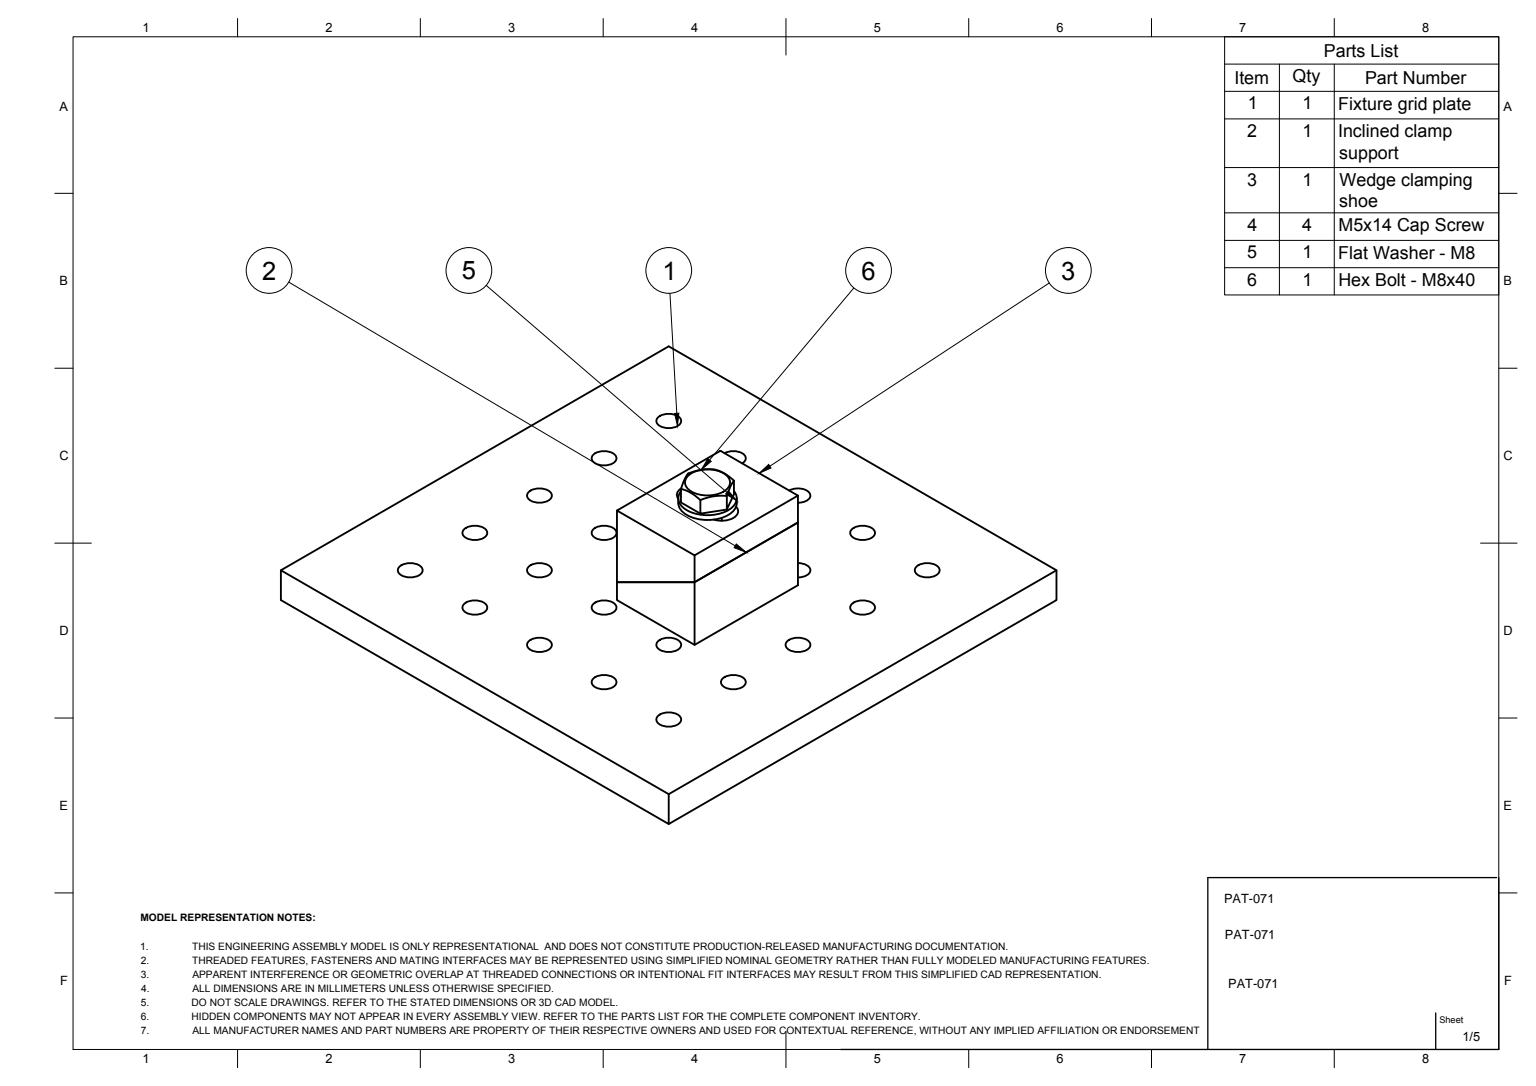
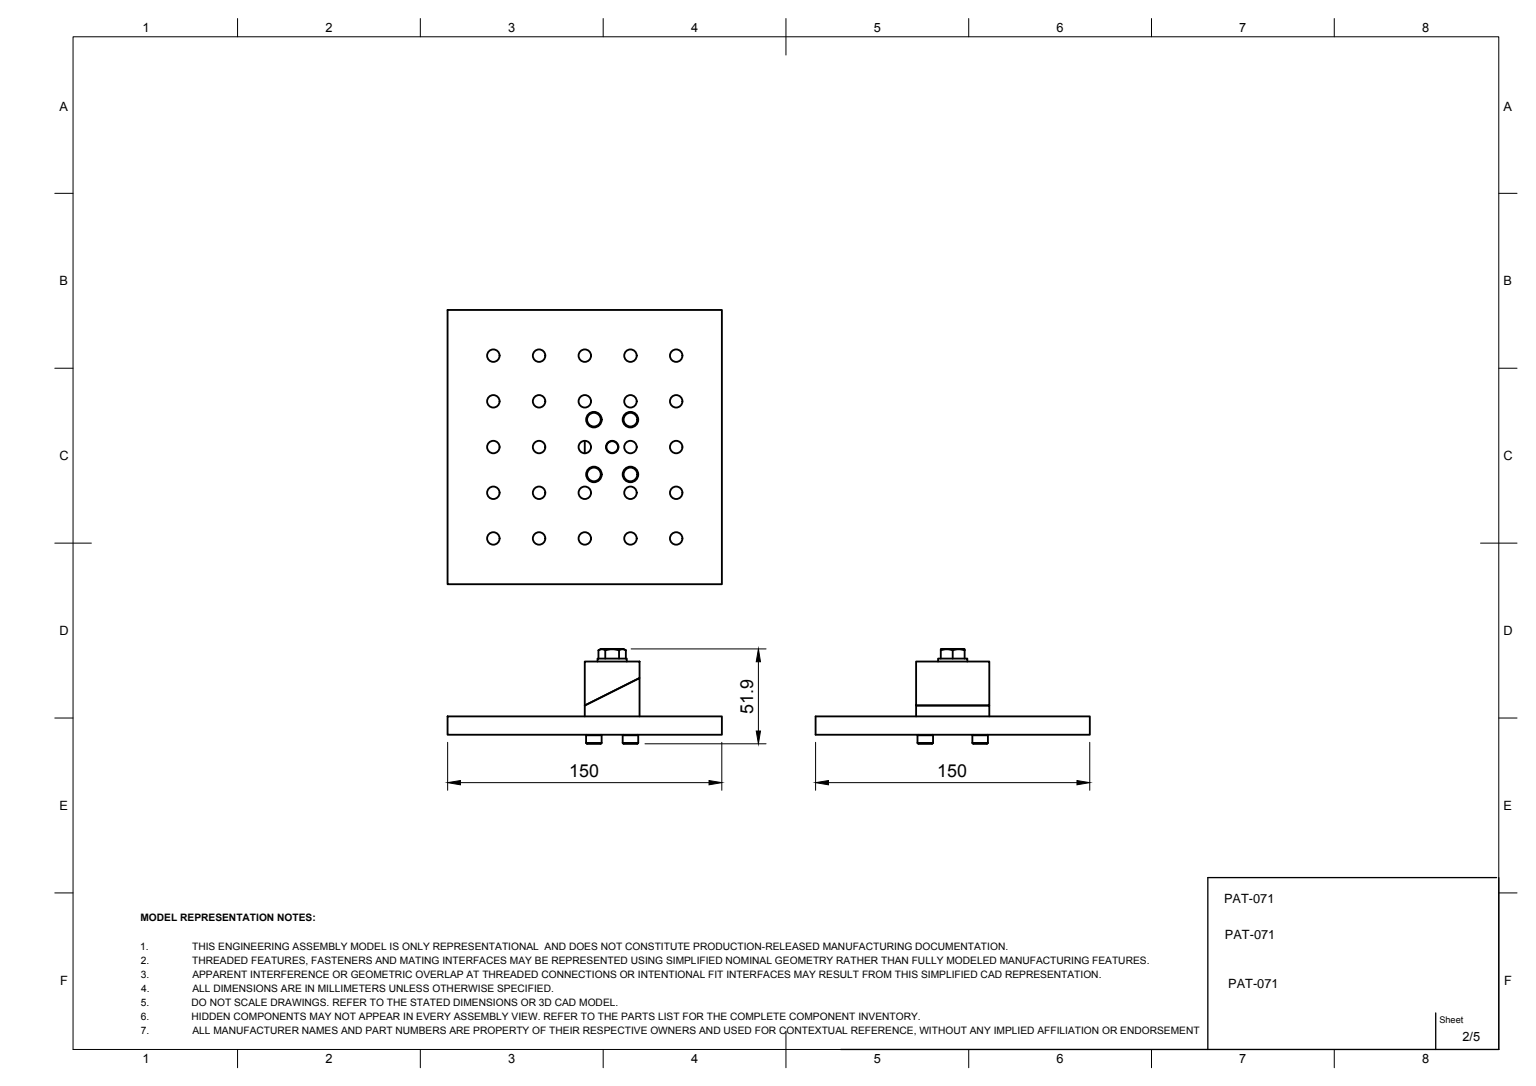
ISO-10303-21;
HEADER;
/* Generated by software containing ST-Developer
 * from STEP Tools, Inc. (www.steptools.com) 
 */

FILE_DESCRIPTION(
/* description */ ('Low-profile wedge edge clamp'),
/* implementation_level */ '2;1');

FILE_NAME(
/* name */ 'PAT-071',
/* time_stamp */ '2026-10-29T15:58:13-07:00',
/* author */ (''),
/* organization */ (''),
/* preprocessor_version */ 'ST-DEVELOPER v20.2',
/* originating_system */ 'Autodesk Translation Framework v15.17.0.0',
/* authorisation */ '');

FILE_SCHEMA (('AUTOMOTIVE_DESIGN { 1 0 10303 214 3 1 1 }'));
ENDSEC;

DATA;
#10=MECHANICAL_DESIGN_GEOMETRIC_PRESENTATION_REPRESENTATION('',(#79,#80,
#81,#82,#83,#84),#2996);
#11=ITEM_DEFINED_TRANSFORMATION($,$,#1784,#1972);
#12=ITEM_DEFINED_TRANSFORMATION($,$,#1881,#1973);
#13=ITEM_DEFINED_TRANSFORMATION($,$,#1907,#1974);
#14=ITEM_DEFINED_TRANSFORMATION($,$,#1922,#1975);
#15=ITEM_DEFINED_TRANSFORMATION($,$,#1922,#1976);
#16=ITEM_DEFINED_TRANSFORMATION($,$,#1922,#1977);
#17=ITEM_DEFINED_TRANSFORMATION($,$,#1922,#1978);
#18=ITEM_DEFINED_TRANSFORMATION($,$,#1946,#1979);
#19=ITEM_DEFINED_TRANSFORMATION($,$,#1955,#1980);
#20=ITEM_DEFINED_TRANSFORMATION($,$,#1783,#1981);
#21=(
REPRESENTATION_RELATIONSHIP($,$,#3029,#3028)
REPRESENTATION_RELATIONSHIP_WITH_TRANSFORMATION(#11)
SHAPE_REPRESENTATION_RELATIONSHIP()
);
#22=(
REPRESENTATION_RELATIONSHIP($,$,#3030,#3028)
REPRESENTATION_RELATIONSHIP_WITH_TRANSFORMATION(#12)
SHAPE_REPRESENTATION_RELATIONSHIP()
);
#23=(
REPRESENTATION_RELATIONSHIP($,$,#3031,#3028)
REPRESENTATION_RELATIONSHIP_WITH_TRANSFORMATION(#13)
SHAPE_REPRESENTATION_RELATIONSHIP()
);
#24=(
REPRESENTATION_RELATIONSHIP($,$,#3032,#3028)
REPRESENTATION_RELATIONSHIP_WITH_TRANSFORMATION(#14)
SHAPE_REPRESENTATION_RELATIONSHIP()
);
#25=(
REPRESENTATION_RELATIONSHIP($,$,#3032,#3028)
REPRESENTATION_RELATIONSHIP_WITH_TRANSFORMATION(#15)
SHAPE_REPRESENTATION_RELATIONSHIP()
);
#26=(
REPRESENTATION_RELATIONSHIP($,$,#3032,#3028)
REPRESENTATION_RELATIONSHIP_WITH_TRANSFORMATION(#16)
SHAPE_REPRESENTATION_RELATIONSHIP()
);
#27=(
REPRESENTATION_RELATIONSHIP($,$,#3032,#3028)
REPRESENTATION_RELATIONSHIP_WITH_TRANSFORMATION(#17)
SHAPE_REPRESENTATION_RELATIONSHIP()
);
#28=(
REPRESENTATION_RELATIONSHIP($,$,#3033,#3028)
REPRESENTATION_RELATIONSHIP_WITH_TRANSFORMATION(#18)
SHAPE_REPRESENTATION_RELATIONSHIP()
);
#29=(
REPRESENTATION_RELATIONSHIP($,$,#3034,#3028)
REPRESENTATION_RELATIONSHIP_WITH_TRANSFORMATION(#19)
SHAPE_REPRESENTATION_RELATIONSHIP()
);
#30=(
REPRESENTATION_RELATIONSHIP($,$,#3028,#3027)
REPRESENTATION_RELATIONSHIP_WITH_TRANSFORMATION(#20)
SHAPE_REPRESENTATION_RELATIONSHIP()
);
#31=CONTEXT_DEPENDENT_SHAPE_REPRESENTATION(#21,#3017);
#32=CONTEXT_DEPENDENT_SHAPE_REPRESENTATION(#22,#3018);
#33=CONTEXT_DEPENDENT_SHAPE_REPRESENTATION(#23,#3019);
#34=CONTEXT_DEPENDENT_SHAPE_REPRESENTATION(#24,#3020);
#35=CONTEXT_DEPENDENT_SHAPE_REPRESENTATION(#25,#3021);
#36=CONTEXT_DEPENDENT_SHAPE_REPRESENTATION(#26,#3022);
#37=CONTEXT_DEPENDENT_SHAPE_REPRESENTATION(#27,#3023);
#38=CONTEXT_DEPENDENT_SHAPE_REPRESENTATION(#28,#3024);
#39=CONTEXT_DEPENDENT_SHAPE_REPRESENTATION(#29,#3025);
#40=CONTEXT_DEPENDENT_SHAPE_REPRESENTATION(#30,#3026);
#41=NEXT_ASSEMBLY_USAGE_OCCURRENCE('Fixture grid plate:1',
'Fixture grid plate:1','Fixture grid plate:1',#3037,#3038,
'Fixture grid plate:1');
#42=NEXT_ASSEMBLY_USAGE_OCCURRENCE('Inclined clamp support:1',
'Inclined clamp support:1','Inclined clamp support:1',#3037,#3039,
'Inclined clamp support:1');
#43=NEXT_ASSEMBLY_USAGE_OCCURRENCE('Wedge clamping shoe:1',
'Wedge clamping shoe:1','Wedge clamping shoe:1',#3037,#3040,
'Wedge clamping shoe:1');
#44=NEXT_ASSEMBLY_USAGE_OCCURRENCE('M5x14 Cap Screw:2',
'M5x14 Cap Screw:2','M5x14 Cap Screw:2',#3037,#3041,'M5x14 Cap Screw:2');
#45=NEXT_ASSEMBLY_USAGE_OCCURRENCE('M5x14 Cap Screw:3',
'M5x14 Cap Screw:3','M5x14 Cap Screw:3',#3037,#3041,'M5x14 Cap Screw:3');
#46=NEXT_ASSEMBLY_USAGE_OCCURRENCE('M5x14 Cap Screw:4',
'M5x14 Cap Screw:4','M5x14 Cap Screw:4',#3037,#3041,'M5x14 Cap Screw:4');
#47=NEXT_ASSEMBLY_USAGE_OCCURRENCE('M5x14 Cap Screw:5',
'M5x14 Cap Screw:5','M5x14 Cap Screw:5',#3037,#3041,'M5x14 Cap Screw:5');
#48=NEXT_ASSEMBLY_USAGE_OCCURRENCE('Flat Washer - M8:2',
'Flat Washer - M8:2','Flat Washer - M8:2',#3037,#3042,
'Flat Washer - M8:2');
#49=NEXT_ASSEMBLY_USAGE_OCCURRENCE('Hex Bolt - M8x40:2',
'Hex Bolt - M8x40:2','Hex Bolt - M8x40:2',#3037,#3043,
'Hex Bolt - M8x40:2');
#50=NEXT_ASSEMBLY_USAGE_OCCURRENCE('Fixture grid and wedge clamp:1',
'Fixture grid and wedge clamp:1','Fixture grid and wedge clamp:1',#3036,
#3037,'Fixture grid and wedge clamp:1');
#51=(
BOUNDED_CURVE()
B_SPLINE_CURVE(2,(#2921,#2922,#2923),.UNSPECIFIED.,.F.,.F.)
B_SPLINE_CURVE_WITH_KNOTS((3,3),(0.14973948338295,0.97160236658079),
 .UNSPECIFIED.)
CURVE()
GEOMETRIC_REPRESENTATION_ITEM()
RATIONAL_B_SPLINE_CURVE((1.07140024848292,1.23714644374248,1.07140024848292))
REPRESENTATION_ITEM('')
);
#52=(
BOUNDED_CURVE()
B_SPLINE_CURVE(2,(#2925,#2926,#2927),.UNSPECIFIED.,.F.,.F.)
B_SPLINE_CURVE_WITH_KNOTS((3,3),(0.14973948338295,0.97160236658079),
 .UNSPECIFIED.)
CURVE()
GEOMETRIC_REPRESENTATION_ITEM()
RATIONAL_B_SPLINE_CURVE((1.07140024848292,1.23714644374248,1.07140024848292))
REPRESENTATION_ITEM('')
);
#53=(
BOUNDED_CURVE()
B_SPLINE_CURVE(2,(#2929,#2930,#2931),.UNSPECIFIED.,.F.,.F.)
B_SPLINE_CURVE_WITH_KNOTS((3,3),(0.14973948338295,0.97160236658079),
 .UNSPECIFIED.)
CURVE()
GEOMETRIC_REPRESENTATION_ITEM()
RATIONAL_B_SPLINE_CURVE((1.07140024848292,1.23714644374248,1.07140024848292))
REPRESENTATION_ITEM('')
);
#54=(
BOUNDED_CURVE()
B_SPLINE_CURVE(2,(#2933,#2934,#2935),.UNSPECIFIED.,.F.,.F.)
B_SPLINE_CURVE_WITH_KNOTS((3,3),(0.149739483382949,0.971602366580789),
 .UNSPECIFIED.)
CURVE()
GEOMETRIC_REPRESENTATION_ITEM()
RATIONAL_B_SPLINE_CURVE((1.07140024848292,1.23714644374248,1.07140024848292))
REPRESENTATION_ITEM('')
);
#55=(
BOUNDED_CURVE()
B_SPLINE_CURVE(2,(#2937,#2938,#2939),.UNSPECIFIED.,.F.,.F.)
B_SPLINE_CURVE_WITH_KNOTS((3,3),(0.14973948338295,0.971602366580789),
 .UNSPECIFIED.)
CURVE()
GEOMETRIC_REPRESENTATION_ITEM()
RATIONAL_B_SPLINE_CURVE((1.07140024848292,1.23714644374248,1.07140024848292))
REPRESENTATION_ITEM('')
);
#56=(
BOUNDED_CURVE()
B_SPLINE_CURVE(2,(#2940,#2941,#2942),.UNSPECIFIED.,.F.,.F.)
B_SPLINE_CURVE_WITH_KNOTS((3,3),(0.14973948338295,0.97160236658079),
 .UNSPECIFIED.)
CURVE()
GEOMETRIC_REPRESENTATION_ITEM()
RATIONAL_B_SPLINE_CURVE((1.07140024848292,1.23714644374248,1.07140024848292))
REPRESENTATION_ITEM('')
);
#57=CONICAL_SURFACE('',#1935,0.4,0.785398163397448);
#58=CONICAL_SURFACE('',#1939,0.41,0.785398163397448);
#59=CONICAL_SURFACE('',#1943,0.26,0.463647609000806);
#60=CONICAL_SURFACE('',#1959,0.36,0.785398163397451);
#61=CONICAL_SURFACE('',#1962,0.734027674973257,1.0471975511966);
#62=ORIENTED_CLOSED_SHELL('',*,#1711,.F.);
#63=BREP_WITH_VOIDS('Body1',#1712,(#62));
#64=ELLIPSE('',#1900,0.475164445218705,0.425);
#65=ELLIPSE('',#1914,0.503115294937453,0.45);
#66=ELLIPSE('',#1916,0.503115294937453,0.45);
#67=SHAPE_REPRESENTATION_RELATIONSHIP('SRR','None',#3029,#73);
#68=SHAPE_REPRESENTATION_RELATIONSHIP('SRR','None',#3030,#74);
#69=SHAPE_REPRESENTATION_RELATIONSHIP('SRR','None',#3031,#75);
#70=SHAPE_REPRESENTATION_RELATIONSHIP('SRR','None',#3032,#76);
#71=SHAPE_REPRESENTATION_RELATIONSHIP('SRR','None',#3033,#77);
#72=SHAPE_REPRESENTATION_RELATIONSHIP('SRR','None',#3034,#78);
#73=ADVANCED_BREP_SHAPE_REPRESENTATION('',(#85),#2990);
#74=ADVANCED_BREP_SHAPE_REPRESENTATION('',(#86),#2991);
#75=ADVANCED_BREP_SHAPE_REPRESENTATION('',(#87),#2992);
#76=ADVANCED_BREP_SHAPE_REPRESENTATION('',(#63),#2993);
#77=ADVANCED_BREP_SHAPE_REPRESENTATION('',(#88),#2994);
#78=ADVANCED_BREP_SHAPE_REPRESENTATION('',(#89),#2995);
#79=STYLED_ITEM('',(#3140),#85);
#80=STYLED_ITEM('',(#3119),#86);
#81=STYLED_ITEM('',(#3140),#87);
#82=STYLED_ITEM('',(#3133),#63);
#83=STYLED_ITEM('',(#3133),#88);
#84=STYLED_ITEM('',(#3133),#89);
#85=MANIFOLD_SOLID_BREP('Body1',#1708);
#86=MANIFOLD_SOLID_BREP('Body1',#1709);
#87=MANIFOLD_SOLID_BREP('Body1',#1710);
#88=MANIFOLD_SOLID_BREP('Body1',#1713);
#89=MANIFOLD_SOLID_BREP('Body1',#1714);
#90=FACE_BOUND('',#336,.T.);
#91=FACE_BOUND('',#337,.T.);
#92=FACE_BOUND('',#338,.T.);
#93=FACE_BOUND('',#339,.T.);
#94=FACE_BOUND('',#340,.T.);
#95=FACE_BOUND('',#341,.T.);
#96=FACE_BOUND('',#342,.T.);
#97=FACE_BOUND('',#343,.T.);
#98=FACE_BOUND('',#344,.T.);
#99=FACE_BOUND('',#345,.T.);
#100=FACE_BOUND('',#346,.T.);
#101=FACE_BOUND('',#347,.T.);
#102=FACE_BOUND('',#348,.T.);
#103=FACE_BOUND('',#349,.T.);
#104=FACE_BOUND('',#350,.T.);
#105=FACE_BOUND('',#351,.T.);
#106=FACE_BOUND('',#352,.T.);
#107=FACE_BOUND('',#353,.T.);
#108=FACE_BOUND('',#354,.T.);
#109=FACE_BOUND('',#355,.T.);
#110=FACE_BOUND('',#356,.T.);
#111=FACE_BOUND('',#357,.T.);
#112=FACE_BOUND('',#358,.T.);
#113=FACE_BOUND('',#359,.T.);
#114=FACE_BOUND('',#360,.T.);
#115=FACE_BOUND('',#361,.T.);
#116=FACE_BOUND('',#362,.T.);
#117=FACE_BOUND('',#363,.T.);
#118=FACE_BOUND('',#364,.T.);
#119=FACE_BOUND('',#365,.T.);
#120=FACE_BOUND('',#367,.T.);
#121=FACE_BOUND('',#368,.T.);
#122=FACE_BOUND('',#369,.T.);
#123=FACE_BOUND('',#370,.T.);
#124=FACE_BOUND('',#371,.T.);
#125=FACE_BOUND('',#372,.T.);
#126=FACE_BOUND('',#373,.T.);
#127=FACE_BOUND('',#374,.T.);
#128=FACE_BOUND('',#375,.T.);
#129=FACE_BOUND('',#376,.T.);
#130=FACE_BOUND('',#377,.T.);
#131=FACE_BOUND('',#378,.T.);
#132=FACE_BOUND('',#379,.T.);
#133=FACE_BOUND('',#380,.T.);
#134=FACE_BOUND('',#381,.T.);
#135=FACE_BOUND('',#382,.T.);
#136=FACE_BOUND('',#383,.T.);
#137=FACE_BOUND('',#384,.T.);
#138=FACE_BOUND('',#385,.T.);
#139=FACE_BOUND('',#386,.T.);
#140=FACE_BOUND('',#387,.T.);
#141=FACE_BOUND('',#388,.T.);
#142=FACE_BOUND('',#389,.T.);
#143=FACE_BOUND('',#390,.T.);
#144=FACE_BOUND('',#391,.T.);
#145=FACE_BOUND('',#392,.T.);
#146=FACE_BOUND('',#393,.T.);
#147=FACE_BOUND('',#394,.T.);
#148=FACE_BOUND('',#395,.T.);
#149=FACE_BOUND('',#396,.T.);
#150=FACE_BOUND('',#408,.T.);
#151=FACE_BOUND('',#409,.T.);
#152=FACE_BOUND('',#410,.T.);
#153=FACE_BOUND('',#411,.T.);
#154=FACE_BOUND('',#412,.T.);
#155=FACE_BOUND('',#415,.T.);
#156=FACE_BOUND('',#421,.T.);
#157=FACE_BOUND('',#426,.T.);
#158=FACE_BOUND('',#444,.T.);
#159=FACE_BOUND('',#450,.T.);
#160=FACE_BOUND('',#452,.T.);
#161=FACE_BOUND('',#465,.T.);
#162=PLANE('',#1875);
#163=PLANE('',#1876);
#164=PLANE('',#1877);
#165=PLANE('',#1878);
#166=PLANE('',#1879);
#167=PLANE('',#1880);
#168=PLANE('',#1885);
#169=PLANE('',#1889);
#170=PLANE('',#1893);
#171=PLANE('',#1897);
#172=PLANE('',#1901);
#173=PLANE('',#1902);
#174=PLANE('',#1903);
#175=PLANE('',#1904);
#176=PLANE('',#1905);
#177=PLANE('',#1906);
#178=PLANE('',#1908);
#179=PLANE('',#1909);
#180=PLANE('',#1910);
#181=PLANE('',#1917);
#182=PLANE('',#1918);
#183=PLANE('',#1919);
#184=PLANE('',#1920);
#185=PLANE('',#1921);
#186=PLANE('',#1923);
#187=PLANE('',#1924);
#188=PLANE('',#1925);
#189=PLANE('',#1926);
#190=PLANE('',#1927);
#191=PLANE('',#1928);
#192=PLANE('',#1929);
#193=PLANE('',#1930);
#194=PLANE('',#1931);
#195=PLANE('',#1933);
#196=PLANE('',#1941);
#197=PLANE('',#1953);
#198=PLANE('',#1954);
#199=PLANE('',#1961);
#200=PLANE('',#1964);
#201=PLANE('',#1965);
#202=PLANE('',#1966);
#203=PLANE('',#1967);
#204=PLANE('',#1968);
#205=PLANE('',#1969);
#206=PLANE('',#1970);
#207=PLANE('',#1971);
#208=FACE_OUTER_BOUND('',#301,.T.);
#209=FACE_OUTER_BOUND('',#302,.T.);
#210=FACE_OUTER_BOUND('',#303,.T.);
#211=FACE_OUTER_BOUND('',#304,.T.);
#212=FACE_OUTER_BOUND('',#305,.T.);
#213=FACE_OUTER_BOUND('',#306,.T.);
#214=FACE_OUTER_BOUND('',#307,.T.);
#215=FACE_OUTER_BOUND('',#308,.T.);
#216=FACE_OUTER_BOUND('',#309,.T.);
#217=FACE_OUTER_BOUND('',#310,.T.);
#218=FACE_OUTER_BOUND('',#311,.T.);
#219=FACE_OUTER_BOUND('',#312,.T.);
#220=FACE_OUTER_BOUND('',#313,.T.);
#221=FACE_OUTER_BOUND('',#314,.T.);
#222=FACE_OUTER_BOUND('',#315,.T.);
#223=FACE_OUTER_BOUND('',#316,.T.);
#224=FACE_OUTER_BOUND('',#317,.T.);
#225=FACE_OUTER_BOUND('',#318,.T.);
#226=FACE_OUTER_BOUND('',#319,.T.);
#227=FACE_OUTER_BOUND('',#320,.T.);
#228=FACE_OUTER_BOUND('',#321,.T.);
#229=FACE_OUTER_BOUND('',#322,.T.);
#230=FACE_OUTER_BOUND('',#323,.T.);
#231=FACE_OUTER_BOUND('',#324,.T.);
#232=FACE_OUTER_BOUND('',#325,.T.);
#233=FACE_OUTER_BOUND('',#326,.T.);
#234=FACE_OUTER_BOUND('',#327,.T.);
#235=FACE_OUTER_BOUND('',#328,.T.);
#236=FACE_OUTER_BOUND('',#329,.T.);
#237=FACE_OUTER_BOUND('',#330,.T.);
#238=FACE_OUTER_BOUND('',#331,.T.);
#239=FACE_OUTER_BOUND('',#332,.T.);
#240=FACE_OUTER_BOUND('',#333,.T.);
#241=FACE_OUTER_BOUND('',#334,.T.);
#242=FACE_OUTER_BOUND('',#335,.T.);
#243=FACE_OUTER_BOUND('',#366,.T.);
#244=FACE_OUTER_BOUND('',#397,.T.);
#245=FACE_OUTER_BOUND('',#398,.T.);
#246=FACE_OUTER_BOUND('',#399,.T.);
#247=FACE_OUTER_BOUND('',#400,.T.);
#248=FACE_OUTER_BOUND('',#401,.T.);
#249=FACE_OUTER_BOUND('',#402,.T.);
#250=FACE_OUTER_BOUND('',#403,.T.);
#251=FACE_OUTER_BOUND('',#404,.T.);
#252=FACE_OUTER_BOUND('',#405,.T.);
#253=FACE_OUTER_BOUND('',#406,.T.);
#254=FACE_OUTER_BOUND('',#407,.T.);
#255=FACE_OUTER_BOUND('',#413,.T.);
#256=FACE_OUTER_BOUND('',#414,.T.);
#257=FACE_OUTER_BOUND('',#416,.T.);
#258=FACE_OUTER_BOUND('',#417,.T.);
#259=FACE_OUTER_BOUND('',#418,.T.);
#260=FACE_OUTER_BOUND('',#419,.T.);
#261=FACE_OUTER_BOUND('',#420,.T.);
#262=FACE_OUTER_BOUND('',#422,.T.);
#263=FACE_OUTER_BOUND('',#423,.T.);
#264=FACE_OUTER_BOUND('',#424,.T.);
#265=FACE_OUTER_BOUND('',#425,.T.);
#266=FACE_OUTER_BOUND('',#427,.T.);
#267=FACE_OUTER_BOUND('',#428,.T.);
#268=FACE_OUTER_BOUND('',#429,.T.);
#269=FACE_OUTER_BOUND('',#430,.T.);
#270=FACE_OUTER_BOUND('',#431,.T.);
#271=FACE_OUTER_BOUND('',#432,.T.);
#272=FACE_OUTER_BOUND('',#433,.T.);
#273=FACE_OUTER_BOUND('',#434,.T.);
#274=FACE_OUTER_BOUND('',#435,.T.);
#275=FACE_OUTER_BOUND('',#436,.T.);
#276=FACE_OUTER_BOUND('',#437,.T.);
#277=FACE_OUTER_BOUND('',#438,.T.);
#278=FACE_OUTER_BOUND('',#439,.T.);
#279=FACE_OUTER_BOUND('',#440,.T.);
#280=FACE_OUTER_BOUND('',#441,.T.);
#281=FACE_OUTER_BOUND('',#442,.T.);
#282=FACE_OUTER_BOUND('',#443,.T.);
#283=FACE_OUTER_BOUND('',#445,.T.);
#284=FACE_OUTER_BOUND('',#446,.T.);
#285=FACE_OUTER_BOUND('',#447,.T.);
#286=FACE_OUTER_BOUND('',#448,.T.);
#287=FACE_OUTER_BOUND('',#449,.T.);
#288=FACE_OUTER_BOUND('',#451,.T.);
#289=FACE_OUTER_BOUND('',#453,.T.);
#290=FACE_OUTER_BOUND('',#454,.T.);
#291=FACE_OUTER_BOUND('',#455,.T.);
#292=FACE_OUTER_BOUND('',#456,.T.);
#293=FACE_OUTER_BOUND('',#457,.T.);
#294=FACE_OUTER_BOUND('',#458,.T.);
#295=FACE_OUTER_BOUND('',#459,.T.);
#296=FACE_OUTER_BOUND('',#460,.T.);
#297=FACE_OUTER_BOUND('',#461,.T.);
#298=FACE_OUTER_BOUND('',#462,.T.);
#299=FACE_OUTER_BOUND('',#463,.T.);
#300=FACE_OUTER_BOUND('',#464,.T.);
#301=EDGE_LOOP('',(#1145,#1146,#1147,#1148));
#302=EDGE_LOOP('',(#1149,#1150,#1151,#1152));
#303=EDGE_LOOP('',(#1153,#1154,#1155,#1156));
#304=EDGE_LOOP('',(#1157,#1158,#1159,#1160));
#305=EDGE_LOOP('',(#1161,#1162,#1163,#1164));
#306=EDGE_LOOP('',(#1165,#1166,#1167,#1168));
#307=EDGE_LOOP('',(#1169,#1170,#1171,#1172));
#308=EDGE_LOOP('',(#1173,#1174,#1175,#1176));
#309=EDGE_LOOP('',(#1177,#1178,#1179,#1180));
#310=EDGE_LOOP('',(#1181,#1182,#1183,#1184));
#311=EDGE_LOOP('',(#1185,#1186,#1187,#1188));
#312=EDGE_LOOP('',(#1189,#1190,#1191,#1192));
#313=EDGE_LOOP('',(#1193,#1194,#1195,#1196));
#314=EDGE_LOOP('',(#1197,#1198,#1199,#1200));
#315=EDGE_LOOP('',(#1201,#1202,#1203,#1204));
#316=EDGE_LOOP('',(#1205,#1206,#1207,#1208));
#317=EDGE_LOOP('',(#1209,#1210,#1211,#1212));
#318=EDGE_LOOP('',(#1213,#1214,#1215,#1216));
#319=EDGE_LOOP('',(#1217,#1218,#1219,#1220));
#320=EDGE_LOOP('',(#1221,#1222,#1223,#1224));
#321=EDGE_LOOP('',(#1225,#1226,#1227,#1228));
#322=EDGE_LOOP('',(#1229,#1230,#1231,#1232));
#323=EDGE_LOOP('',(#1233,#1234,#1235,#1236));
#324=EDGE_LOOP('',(#1237,#1238,#1239,#1240));
#325=EDGE_LOOP('',(#1241,#1242,#1243,#1244));
#326=EDGE_LOOP('',(#1245,#1246,#1247,#1248));
#327=EDGE_LOOP('',(#1249,#1250,#1251,#1252));
#328=EDGE_LOOP('',(#1253,#1254,#1255,#1256));
#329=EDGE_LOOP('',(#1257,#1258,#1259,#1260));
#330=EDGE_LOOP('',(#1261,#1262,#1263,#1264));
#331=EDGE_LOOP('',(#1265,#1266,#1267,#1268));
#332=EDGE_LOOP('',(#1269,#1270,#1271,#1272));
#333=EDGE_LOOP('',(#1273,#1274,#1275,#1276));
#334=EDGE_LOOP('',(#1277,#1278,#1279,#1280));
#335=EDGE_LOOP('',(#1281,#1282,#1283,#1284));
#336=EDGE_LOOP('',(#1285));
#337=EDGE_LOOP('',(#1286));
#338=EDGE_LOOP('',(#1287));
#339=EDGE_LOOP('',(#1288));
#340=EDGE_LOOP('',(#1289));
#341=EDGE_LOOP('',(#1290));
#342=EDGE_LOOP('',(#1291));
#343=EDGE_LOOP('',(#1292));
#344=EDGE_LOOP('',(#1293));
#345=EDGE_LOOP('',(#1294));
#346=EDGE_LOOP('',(#1295));
#347=EDGE_LOOP('',(#1296));
#348=EDGE_LOOP('',(#1297));
#349=EDGE_LOOP('',(#1298));
#350=EDGE_LOOP('',(#1299));
#351=EDGE_LOOP('',(#1300));
#352=EDGE_LOOP('',(#1301));
#353=EDGE_LOOP('',(#1302));
#354=EDGE_LOOP('',(#1303));
#355=EDGE_LOOP('',(#1304));
#356=EDGE_LOOP('',(#1305));
#357=EDGE_LOOP('',(#1306));
#358=EDGE_LOOP('',(#1307));
#359=EDGE_LOOP('',(#1308));
#360=EDGE_LOOP('',(#1309));
#361=EDGE_LOOP('',(#1310));
#362=EDGE_LOOP('',(#1311));
#363=EDGE_LOOP('',(#1312));
#364=EDGE_LOOP('',(#1313));
#365=EDGE_LOOP('',(#1314));
#366=EDGE_LOOP('',(#1315,#1316,#1317,#1318));
#367=EDGE_LOOP('',(#1319));
#368=EDGE_LOOP('',(#1320));
#369=EDGE_LOOP('',(#1321));
#370=EDGE_LOOP('',(#1322));
#371=EDGE_LOOP('',(#1323));
#372=EDGE_LOOP('',(#1324));
#373=EDGE_LOOP('',(#1325));
#374=EDGE_LOOP('',(#1326));
#375=EDGE_LOOP('',(#1327));
#376=EDGE_LOOP('',(#1328));
#377=EDGE_LOOP('',(#1329));
#378=EDGE_LOOP('',(#1330));
#379=EDGE_LOOP('',(#1331));
#380=EDGE_LOOP('',(#1332));
#381=EDGE_LOOP('',(#1333));
#382=EDGE_LOOP('',(#1334));
#383=EDGE_LOOP('',(#1335));
#384=EDGE_LOOP('',(#1336));
#385=EDGE_LOOP('',(#1337));
#386=EDGE_LOOP('',(#1338));
#387=EDGE_LOOP('',(#1339));
#388=EDGE_LOOP('',(#1340));
#389=EDGE_LOOP('',(#1341));
#390=EDGE_LOOP('',(#1342));
#391=EDGE_LOOP('',(#1343));
#392=EDGE_LOOP('',(#1344));
#393=EDGE_LOOP('',(#1345));
#394=EDGE_LOOP('',(#1346));
#395=EDGE_LOOP('',(#1347));
#396=EDGE_LOOP('',(#1348));
#397=EDGE_LOOP('',(#1349,#1350,#1351,#1352));
#398=EDGE_LOOP('',(#1353));
#399=EDGE_LOOP('',(#1354,#1355,#1356,#1357));
#400=EDGE_LOOP('',(#1358));
#401=EDGE_LOOP('',(#1359,#1360,#1361,#1362));
#402=EDGE_LOOP('',(#1363));
#403=EDGE_LOOP('',(#1364,#1365,#1366,#1367));
#404=EDGE_LOOP('',(#1368));
#405=EDGE_LOOP('',(#1369,#1370,#1371,#1372));
#406=EDGE_LOOP('',(#1373,#1374,#1375,#1376));
#407=EDGE_LOOP('',(#1377,#1378,#1379,#1380));
#408=EDGE_LOOP('',(#1381));
#409=EDGE_LOOP('',(#1382));
#410=EDGE_LOOP('',(#1383));
#411=EDGE_LOOP('',(#1384));
#412=EDGE_LOOP('',(#1385));
#413=EDGE_LOOP('',(#1386,#1387,#1388,#1389));
#414=EDGE_LOOP('',(#1390,#1391,#1392,#1393));
#415=EDGE_LOOP('',(#1394));
#416=EDGE_LOOP('',(#1395,#1396,#1397,#1398));
#417=EDGE_LOOP('',(#1399,#1400,#1401,#1402));
#418=EDGE_LOOP('',(#1403,#1404,#1405,#1406));
#419=EDGE_LOOP('',(#1407,#1408,#1409,#1410));
#420=EDGE_LOOP('',(#1411,#1412,#1413,#1414));
#421=EDGE_LOOP('',(#1415,#1416,#1417,#1418));
#422=EDGE_LOOP('',(#1419,#1420,#1421,#1422));
#423=EDGE_LOOP('',(#1423,#1424,#1425,#1426));
#424=EDGE_LOOP('',(#1427,#1428,#1429,#1430));
#425=EDGE_LOOP('',(#1431,#1432,#1433,#1434));
#426=EDGE_LOOP('',(#1435,#1436,#1437,#1438));
#427=EDGE_LOOP('',(#1439,#1440,#1441,#1442));
#428=EDGE_LOOP('',(#1443,#1444,#1445,#1446));
#429=EDGE_LOOP('',(#1447,#1448,#1449,#1450));
#430=EDGE_LOOP('',(#1451,#1452,#1453,#1454));
#431=EDGE_LOOP('',(#1455,#1456,#1457,#1458));
#432=EDGE_LOOP('',(#1459,#1460,#1461,#1462));
#433=EDGE_LOOP('',(#1463,#1464,#1465,#1466));
#434=EDGE_LOOP('',(#1467,#1468,#1469,#1470));
#435=EDGE_LOOP('',(#1471,#1472,#1473,#1474));
#436=EDGE_LOOP('',(#1475,#1476,#1477,#1478,#1479,#1480));
#437=EDGE_LOOP('',(#1481,#1482,#1483,#1484,#1485,#1486));
#438=EDGE_LOOP('',(#1487));
#439=EDGE_LOOP('',(#1488));
#440=EDGE_LOOP('',(#1489,#1490,#1491,#1492));
#441=EDGE_LOOP('',(#1493,#1494,#1495,#1496));
#442=EDGE_LOOP('',(#1497,#1498,#1499,#1500));
#443=EDGE_LOOP('',(#1501));
#444=EDGE_LOOP('',(#1502));
#445=EDGE_LOOP('',(#1503,#1504,#1505,#1506));
#446=EDGE_LOOP('',(#1507,#1508,#1509,#1510));
#447=EDGE_LOOP('',(#1511,#1512,#1513,#1514));
#448=EDGE_LOOP('',(#1515,#1516,#1517,#1518));
#449=EDGE_LOOP('',(#1519));
#450=EDGE_LOOP('',(#1520));
#451=EDGE_LOOP('',(#1521));
#452=EDGE_LOOP('',(#1522));
#453=EDGE_LOOP('',(#1523,#1524,#1525,#1526));
#454=EDGE_LOOP('',(#1527,#1528,#1529,#1530));
#455=EDGE_LOOP('',(#1531));
#456=EDGE_LOOP('',(#1532,#1533,#1534,#1535,#1536,#1537,#1538,#1539,#1540));
#457=EDGE_LOOP('',(#1541,#1542,#1543,#1544));
#458=EDGE_LOOP('',(#1545,#1546,#1547,#1548));
#459=EDGE_LOOP('',(#1549,#1550,#1551,#1552));
#460=EDGE_LOOP('',(#1553,#1554,#1555,#1556));
#461=EDGE_LOOP('',(#1557,#1558,#1559,#1560));
#462=EDGE_LOOP('',(#1561,#1562,#1563,#1564));
#463=EDGE_LOOP('',(#1565));
#464=EDGE_LOOP('',(#1566,#1567,#1568,#1569,#1570,#1571));
#465=EDGE_LOOP('',(#1572));
#466=LINE('',#2508,#585);
#467=LINE('',#2514,#586);
#468=LINE('',#2520,#587);
#469=LINE('',#2526,#588);
#470=LINE('',#2532,#589);
#471=LINE('',#2538,#590);
#472=LINE('',#2544,#591);
#473=LINE('',#2550,#592);
#474=LINE('',#2556,#593);
#475=LINE('',#2562,#594);
#476=LINE('',#2568,#595);
#477=LINE('',#2574,#596);
#478=LINE('',#2580,#597);
#479=LINE('',#2586,#598);
#480=LINE('',#2592,#599);
#481=LINE('',#2598,#600);
#482=LINE('',#2604,#601);
#483=LINE('',#2610,#602);
#484=LINE('',#2616,#603);
#485=LINE('',#2622,#604);
#486=LINE('',#2628,#605);
#487=LINE('',#2634,#606);
#488=LINE('',#2640,#607);
#489=LINE('',#2646,#608);
#490=LINE('',#2652,#609);
#491=LINE('',#2658,#610);
#492=LINE('',#2664,#611);
#493=LINE('',#2670,#612);
#494=LINE('',#2676,#613);
#495=LINE('',#2682,#614);
#496=LINE('',#2687,#615);
#497=LINE('',#2689,#616);
#498=LINE('',#2691,#617);
#499=LINE('',#2692,#618);
#500=LINE('',#2695,#619);
#501=LINE('',#2697,#620);
#502=LINE('',#2698,#621);
#503=LINE('',#2701,#622);
#504=LINE('',#2703,#623);
#505=LINE('',#2704,#624);
#506=LINE('',#2706,#625);
#507=LINE('',#2707,#626);
#508=LINE('',#2715,#627);
#509=LINE('',#2722,#628);
#510=LINE('',#2729,#629);
#511=LINE('',#2736,#630);
#512=LINE('',#2743,#631);
#513=LINE('',#2748,#632);
#514=LINE('',#2750,#633);
#515=LINE('',#2752,#634);
#516=LINE('',#2753,#635);
#517=LINE('',#2756,#636);
#518=LINE('',#2758,#637);
#519=LINE('',#2759,#638);
#520=LINE('',#2762,#639);
#521=LINE('',#2764,#640);
#522=LINE('',#2765,#641);
#523=LINE('',#2767,#642);
#524=LINE('',#2768,#643);
#525=LINE('',#2775,#644);
#526=LINE('',#2777,#645);
#527=LINE('',#2779,#646);
#528=LINE('',#2780,#647);
#529=LINE('',#2784,#648);
#530=LINE('',#2786,#649);
#531=LINE('',#2788,#650);
#532=LINE('',#2789,#651);
#533=LINE('',#2793,#652);
#534=LINE('',#2795,#653);
#535=LINE('',#2797,#654);
#536=LINE('',#2798,#655);
#537=LINE('',#2807,#656);
#538=LINE('',#2809,#657);
#539=LINE('',#2810,#658);
#540=LINE('',#2813,#659);
#541=LINE('',#2815,#660);
#542=LINE('',#2816,#661);
#543=LINE('',#2818,#662);
#544=LINE('',#2819,#663);
#545=LINE('',#2826,#664);
#546=LINE('',#2828,#665);
#547=LINE('',#2830,#666);
#548=LINE('',#2831,#667);
#549=LINE('',#2834,#668);
#550=LINE('',#2836,#669);
#551=LINE('',#2837,#670);
#552=LINE('',#2840,#671);
#553=LINE('',#2842,#672);
#554=LINE('',#2843,#673);
#555=LINE('',#2846,#674);
#556=LINE('',#2848,#675);
#557=LINE('',#2849,#676);
#558=LINE('',#2852,#677);
#559=LINE('',#2854,#678);
#560=LINE('',#2855,#679);
#561=LINE('',#2857,#680);
#562=LINE('',#2858,#681);
#563=LINE('',#2870,#682);
#564=LINE('',#2874,#683);
#565=LINE('',#2878,#684);
#566=LINE('',#2885,#685);
#567=LINE('',#2887,#686);
#568=LINE('',#2893,#687);
#569=LINE('',#2899,#688);
#570=LINE('',#2908,#689);
#571=LINE('',#2913,#690);
#572=LINE('',#2919,#691);
#573=LINE('',#2945,#692);
#574=LINE('',#2947,#693);
#575=LINE('',#2948,#694);
#576=LINE('',#2951,#695);
#577=LINE('',#2952,#696);
#578=LINE('',#2955,#697);
#579=LINE('',#2956,#698);
#580=LINE('',#2959,#699);
#581=LINE('',#2960,#700);
#582=LINE('',#2963,#701);
#583=LINE('',#2964,#702);
#584=LINE('',#2966,#703);
#585=VECTOR('',#1992,0.275);
#586=VECTOR('',#1999,0.275);
#587=VECTOR('',#2006,0.275);
#588=VECTOR('',#2013,0.275);
#589=VECTOR('',#2020,0.34);
#590=VECTOR('',#2027,0.34);
#591=VECTOR('',#2034,0.34);
#592=VECTOR('',#2041,0.34);
#593=VECTOR('',#2048,0.34);
#594=VECTOR('',#2055,0.34);
#595=VECTOR('',#2062,0.34);
#596=VECTOR('',#2069,0.34);
#597=VECTOR('',#2076,0.34);
#598=VECTOR('',#2083,0.34);
#599=VECTOR('',#2090,0.34);
#600=VECTOR('',#2097,0.34);
#601=VECTOR('',#2104,0.34);
#602=VECTOR('',#2111,0.34);
#603=VECTOR('',#2118,0.34);
#604=VECTOR('',#2125,0.34);
#605=VECTOR('',#2132,0.34);
#606=VECTOR('',#2139,0.34);
#607=VECTOR('',#2146,0.34);
#608=VECTOR('',#2153,0.34);
#609=VECTOR('',#2160,0.34);
#610=VECTOR('',#2167,0.34);
#611=VECTOR('',#2174,0.34);
#612=VECTOR('',#2181,0.34);
#613=VECTOR('',#2188,0.34);
#614=VECTOR('',#2195,0.34);
#615=VECTOR('',#2200,1.);
#616=VECTOR('',#2201,1.);
#617=VECTOR('',#2202,1.);
#618=VECTOR('',#2203,1.);
#619=VECTOR('',#2206,1.);
#620=VECTOR('',#2207,1.);
#621=VECTOR('',#2208,1.);
#622=VECTOR('',#2211,1.);
#623=VECTOR('',#2212,1.);
#624=VECTOR('',#2213,1.);
#625=VECTOR('',#2216,1.);
#626=VECTOR('',#2217,1.);
#627=VECTOR('',#2228,0.21);
#628=VECTOR('',#2237,0.21);
#629=VECTOR('',#2246,0.21);
#630=VECTOR('',#2255,0.21);
#631=VECTOR('',#2264,0.425);
#632=VECTOR('',#2269,1.);
#633=VECTOR('',#2270,1.);
#634=VECTOR('',#2271,1.);
#635=VECTOR('',#2272,1.);
#636=VECTOR('',#2275,1.);
#637=VECTOR('',#2276,1.);
#638=VECTOR('',#2277,1.);
#639=VECTOR('',#2280,1.);
#640=VECTOR('',#2281,1.);
#641=VECTOR('',#2282,1.);
#642=VECTOR('',#2285,1.);
#643=VECTOR('',#2286,1.);
#644=VECTOR('',#2295,1.);
#645=VECTOR('',#2296,1.);
#646=VECTOR('',#2297,1.);
#647=VECTOR('',#2298,1.);
#648=VECTOR('',#2301,1.);
#649=VECTOR('',#2302,1.);
#650=VECTOR('',#2303,1.);
#651=VECTOR('',#2304,1.);
#652=VECTOR('',#2307,1.);
#653=VECTOR('',#2308,1.);
#654=VECTOR('',#2309,1.);
#655=VECTOR('',#2310,1.);
#656=VECTOR('',#2325,1.);
#657=VECTOR('',#2326,1.);
#658=VECTOR('',#2327,1.);
#659=VECTOR('',#2330,1.);
#660=VECTOR('',#2331,1.);
#661=VECTOR('',#2332,1.);
#662=VECTOR('',#2335,1.);
#663=VECTOR('',#2336,1.);
#664=VECTOR('',#2345,1.);
#665=VECTOR('',#2346,1.);
#666=VECTOR('',#2347,1.);
#667=VECTOR('',#2348,1.);
#668=VECTOR('',#2351,1.);
#669=VECTOR('',#2352,1.);
#670=VECTOR('',#2353,1.);
#671=VECTOR('',#2356,1.);
#672=VECTOR('',#2357,1.);
#673=VECTOR('',#2358,1.);
#674=VECTOR('',#2361,1.);
#675=VECTOR('',#2362,1.);
#676=VECTOR('',#2363,1.);
#677=VECTOR('',#2366,1.);
#678=VECTOR('',#2367,1.);
#679=VECTOR('',#2368,1.);
#680=VECTOR('',#2371,1.);
#681=VECTOR('',#2372,1.);
#682=VECTOR('',#2389,0.4);
#683=VECTOR('',#2394,0.425);
#684=VECTOR('',#2399,0.41);
#685=VECTOR('',#2408,0.26);
#686=VECTOR('',#2411,0.25);
#687=VECTOR('',#2418,0.42);
#688=VECTOR('',#2425,0.8);
#689=VECTOR('',#2438,0.4);
#690=VECTOR('',#2445,0.36);
#691=VECTOR('',#2452,0.734027674973257);
#692=VECTOR('',#2455,1.);
#693=VECTOR('',#2456,1.);
#694=VECTOR('',#2457,1.);
#695=VECTOR('',#2460,1.);
#696=VECTOR('',#2461,1.);
#697=VECTOR('',#2464,1.);
#698=VECTOR('',#2465,1.);
#699=VECTOR('',#2468,1.);
#700=VECTOR('',#2469,1.);
#701=VECTOR('',#2472,1.);
#702=VECTOR('',#2473,1.);
#703=VECTOR('',#2476,1.);
#704=CIRCLE('',#1786,0.275);
#705=CIRCLE('',#1787,0.275);
#706=CIRCLE('',#1789,0.275);
#707=CIRCLE('',#1790,0.275);
#708=CIRCLE('',#1792,0.275);
#709=CIRCLE('',#1793,0.275);
#710=CIRCLE('',#1795,0.275);
#711=CIRCLE('',#1796,0.275);
#712=CIRCLE('',#1798,0.34);
#713=CIRCLE('',#1799,0.34);
#714=CIRCLE('',#1801,0.34);
#715=CIRCLE('',#1802,0.34);
#716=CIRCLE('',#1804,0.34);
#717=CIRCLE('',#1805,0.34);
#718=CIRCLE('',#1807,0.34);
#719=CIRCLE('',#1808,0.34);
#720=CIRCLE('',#1810,0.34);
#721=CIRCLE('',#1811,0.34);
#722=CIRCLE('',#1813,0.34);
#723=CIRCLE('',#1814,0.34);
#724=CIRCLE('',#1816,0.34);
#725=CIRCLE('',#1817,0.34);
#726=CIRCLE('',#1819,0.34);
#727=CIRCLE('',#1820,0.34);
#728=CIRCLE('',#1822,0.34);
#729=CIRCLE('',#1823,0.34);
#730=CIRCLE('',#1825,0.34);
#731=CIRCLE('',#1826,0.34);
#732=CIRCLE('',#1828,0.34);
#733=CIRCLE('',#1829,0.34);
#734=CIRCLE('',#1831,0.34);
#735=CIRCLE('',#1832,0.34);
#736=CIRCLE('',#1834,0.34);
#737=CIRCLE('',#1835,0.34);
#738=CIRCLE('',#1837,0.34);
#739=CIRCLE('',#1838,0.34);
#740=CIRCLE('',#1840,0.34);
#741=CIRCLE('',#1841,0.34);
#742=CIRCLE('',#1843,0.34);
#743=CIRCLE('',#1844,0.34);
#744=CIRCLE('',#1846,0.34);
#745=CIRCLE('',#1847,0.34);
#746=CIRCLE('',#1849,0.34);
#747=CIRCLE('',#1850,0.34);
#748=CIRCLE('',#1852,0.34);
#749=CIRCLE('',#1853,0.34);
#750=CIRCLE('',#1855,0.34);
#751=CIRCLE('',#1856,0.34);
#752=CIRCLE('',#1858,0.34);
#753=CIRCLE('',#1859,0.34);
#754=CIRCLE('',#1861,0.34);
#755=CIRCLE('',#1862,0.34);
#756=CIRCLE('',#1864,0.34);
#757=CIRCLE('',#1865,0.34);
#758=CIRCLE('',#1867,0.34);
#759=CIRCLE('',#1868,0.34);
#760=CIRCLE('',#1870,0.34);
#761=CIRCLE('',#1871,0.34);
#762=CIRCLE('',#1873,0.34);
#763=CIRCLE('',#1874,0.34);
#764=CIRCLE('',#1883,0.21);
#765=CIRCLE('',#1884,0.21);
#766=CIRCLE('',#1887,0.21);
#767=CIRCLE('',#1888,0.21);
#768=CIRCLE('',#1891,0.21);
#769=CIRCLE('',#1892,0.21);
#770=CIRCLE('',#1895,0.21);
#771=CIRCLE('',#1896,0.21);
#772=CIRCLE('',#1899,0.425);
#773=CIRCLE('',#1911,0.45);
#774=CIRCLE('',#1912,0.45);
#775=CIRCLE('',#1932,0.24505);
#776=CIRCLE('',#1934,0.375);
#777=CIRCLE('',#1936,0.425);
#778=CIRCLE('',#1938,0.425);
#779=CIRCLE('',#1940,0.395);
#780=CIRCLE('',#1942,0.27);
#781=CIRCLE('',#1944,0.24505);
#782=CIRCLE('',#1948,0.42);
#783=CIRCLE('',#1949,0.42);
#784=CIRCLE('',#1951,0.8);
#785=CIRCLE('',#1952,0.8);
#786=CIRCLE('',#1957,0.3933);
#787=CIRCLE('',#1958,0.3933);
#788=CIRCLE('',#1960,0.32);
#789=CIRCLE('',#1963,0.6175);
#790=VERTEX_POINT('',#2505);
#791=VERTEX_POINT('',#2507);
#792=VERTEX_POINT('',#2511);
#793=VERTEX_POINT('',#2513);
#794=VERTEX_POINT('',#2517);
#795=VERTEX_POINT('',#2519);
#796=VERTEX_POINT('',#2523);
#797=VERTEX_POINT('',#2525);
#798=VERTEX_POINT('',#2529);
#799=VERTEX_POINT('',#2531);
#800=VERTEX_POINT('',#2535);
#801=VERTEX_POINT('',#2537);
#802=VERTEX_POINT('',#2541);
#803=VERTEX_POINT('',#2543);
#804=VERTEX_POINT('',#2547);
#805=VERTEX_POINT('',#2549);
#806=VERTEX_POINT('',#2553);
#807=VERTEX_POINT('',#2555);
#808=VERTEX_POINT('',#2559);
#809=VERTEX_POINT('',#2561);
#810=VERTEX_POINT('',#2565);
#811=VERTEX_POINT('',#2567);
#812=VERTEX_POINT('',#2571);
#813=VERTEX_POINT('',#2573);
#814=VERTEX_POINT('',#2577);
#815=VERTEX_POINT('',#2579);
#816=VERTEX_POINT('',#2583);
#817=VERTEX_POINT('',#2585);
#818=VERTEX_POINT('',#2589);
#819=VERTEX_POINT('',#2591);
#820=VERTEX_POINT('',#2595);
#821=VERTEX_POINT('',#2597);
#822=VERTEX_POINT('',#2601);
#823=VERTEX_POINT('',#2603);
#824=VERTEX_POINT('',#2607);
#825=VERTEX_POINT('',#2609);
#826=VERTEX_POINT('',#2613);
#827=VERTEX_POINT('',#2615);
#828=VERTEX_POINT('',#2619);
#829=VERTEX_POINT('',#2621);
#830=VERTEX_POINT('',#2625);
#831=VERTEX_POINT('',#2627);
#832=VERTEX_POINT('',#2631);
#833=VERTEX_POINT('',#2633);
#834=VERTEX_POINT('',#2637);
#835=VERTEX_POINT('',#2639);
#836=VERTEX_POINT('',#2643);
#837=VERTEX_POINT('',#2645);
#838=VERTEX_POINT('',#2649);
#839=VERTEX_POINT('',#2651);
#840=VERTEX_POINT('',#2655);
#841=VERTEX_POINT('',#2657);
#842=VERTEX_POINT('',#2661);
#843=VERTEX_POINT('',#2663);
#844=VERTEX_POINT('',#2667);
#845=VERTEX_POINT('',#2669);
#846=VERTEX_POINT('',#2673);
#847=VERTEX_POINT('',#2675);
#848=VERTEX_POINT('',#2679);
#849=VERTEX_POINT('',#2681);
#850=VERTEX_POINT('',#2685);
#851=VERTEX_POINT('',#2686);
#852=VERTEX_POINT('',#2688);
#853=VERTEX_POINT('',#2690);
#854=VERTEX_POINT('',#2694);
#855=VERTEX_POINT('',#2696);
#856=VERTEX_POINT('',#2700);
#857=VERTEX_POINT('',#2702);
#858=VERTEX_POINT('',#2712);
#859=VERTEX_POINT('',#2714);
#860=VERTEX_POINT('',#2719);
#861=VERTEX_POINT('',#2721);
#862=VERTEX_POINT('',#2726);
#863=VERTEX_POINT('',#2728);
#864=VERTEX_POINT('',#2733);
#865=VERTEX_POINT('',#2735);
#866=VERTEX_POINT('',#2740);
#867=VERTEX_POINT('',#2742);
#868=VERTEX_POINT('',#2746);
#869=VERTEX_POINT('',#2747);
#870=VERTEX_POINT('',#2749);
#871=VERTEX_POINT('',#2751);
#872=VERTEX_POINT('',#2755);
#873=VERTEX_POINT('',#2757);
#874=VERTEX_POINT('',#2761);
#875=VERTEX_POINT('',#2763);
#876=VERTEX_POINT('',#2773);
#877=VERTEX_POINT('',#2774);
#878=VERTEX_POINT('',#2776);
#879=VERTEX_POINT('',#2778);
#880=VERTEX_POINT('',#2782);
#881=VERTEX_POINT('',#2783);
#882=VERTEX_POINT('',#2785);
#883=VERTEX_POINT('',#2787);
#884=VERTEX_POINT('',#2791);
#885=VERTEX_POINT('',#2792);
#886=VERTEX_POINT('',#2794);
#887=VERTEX_POINT('',#2796);
#888=VERTEX_POINT('',#2806);
#889=VERTEX_POINT('',#2808);
#890=VERTEX_POINT('',#2812);
#891=VERTEX_POINT('',#2814);
#892=VERTEX_POINT('',#2824);
#893=VERTEX_POINT('',#2825);
#894=VERTEX_POINT('',#2827);
#895=VERTEX_POINT('',#2829);
#896=VERTEX_POINT('',#2833);
#897=VERTEX_POINT('',#2835);
#898=VERTEX_POINT('',#2839);
#899=VERTEX_POINT('',#2841);
#900=VERTEX_POINT('',#2845);
#901=VERTEX_POINT('',#2847);
#902=VERTEX_POINT('',#2851);
#903=VERTEX_POINT('',#2853);
#904=VERTEX_POINT('',#2862);
#905=VERTEX_POINT('',#2865);
#906=VERTEX_POINT('',#2868);
#907=VERTEX_POINT('',#2872);
#908=VERTEX_POINT('',#2876);
#909=VERTEX_POINT('',#2880);
#910=VERTEX_POINT('',#2883);
#911=VERTEX_POINT('',#2890);
#912=VERTEX_POINT('',#2892);
#913=VERTEX_POINT('',#2896);
#914=VERTEX_POINT('',#2898);
#915=VERTEX_POINT('',#2905);
#916=VERTEX_POINT('',#2907);
#917=VERTEX_POINT('',#2911);
#918=VERTEX_POINT('',#2916);
#919=VERTEX_POINT('',#2918);
#920=VERTEX_POINT('',#2920);
#921=VERTEX_POINT('',#2924);
#922=VERTEX_POINT('',#2928);
#923=VERTEX_POINT('',#2932);
#924=VERTEX_POINT('',#2936);
#925=VERTEX_POINT('',#2944);
#926=VERTEX_POINT('',#2946);
#927=VERTEX_POINT('',#2950);
#928=VERTEX_POINT('',#2954);
#929=VERTEX_POINT('',#2958);
#930=VERTEX_POINT('',#2962);
#931=EDGE_CURVE('',#790,#790,#704,.T.);
#932=EDGE_CURVE('',#790,#791,#466,.T.);
#933=EDGE_CURVE('',#791,#791,#705,.T.);
#934=EDGE_CURVE('',#792,#792,#706,.T.);
#935=EDGE_CURVE('',#792,#793,#467,.T.);
#936=EDGE_CURVE('',#793,#793,#707,.T.);
#937=EDGE_CURVE('',#794,#794,#708,.T.);
#938=EDGE_CURVE('',#794,#795,#468,.T.);
#939=EDGE_CURVE('',#795,#795,#709,.T.);
#940=EDGE_CURVE('',#796,#796,#710,.T.);
#941=EDGE_CURVE('',#796,#797,#469,.T.);
#942=EDGE_CURVE('',#797,#797,#711,.T.);
#943=EDGE_CURVE('',#798,#798,#712,.T.);
#944=EDGE_CURVE('',#798,#799,#470,.T.);
#945=EDGE_CURVE('',#799,#799,#713,.T.);
#946=EDGE_CURVE('',#800,#800,#714,.T.);
#947=EDGE_CURVE('',#800,#801,#471,.T.);
#948=EDGE_CURVE('',#801,#801,#715,.T.);
#949=EDGE_CURVE('',#802,#802,#716,.T.);
#950=EDGE_CURVE('',#802,#803,#472,.T.);
#951=EDGE_CURVE('',#803,#803,#717,.T.);
#952=EDGE_CURVE('',#804,#804,#718,.T.);
#953=EDGE_CURVE('',#804,#805,#473,.T.);
#954=EDGE_CURVE('',#805,#805,#719,.T.);
#955=EDGE_CURVE('',#806,#806,#720,.T.);
#956=EDGE_CURVE('',#806,#807,#474,.T.);
#957=EDGE_CURVE('',#807,#807,#721,.T.);
#958=EDGE_CURVE('',#808,#808,#722,.T.);
#959=EDGE_CURVE('',#808,#809,#475,.T.);
#960=EDGE_CURVE('',#809,#809,#723,.T.);
#961=EDGE_CURVE('',#810,#810,#724,.T.);
#962=EDGE_CURVE('',#810,#811,#476,.T.);
#963=EDGE_CURVE('',#811,#811,#725,.T.);
#964=EDGE_CURVE('',#812,#812,#726,.T.);
#965=EDGE_CURVE('',#812,#813,#477,.T.);
#966=EDGE_CURVE('',#813,#813,#727,.T.);
#967=EDGE_CURVE('',#814,#814,#728,.T.);
#968=EDGE_CURVE('',#814,#815,#478,.T.);
#969=EDGE_CURVE('',#815,#815,#729,.T.);
#970=EDGE_CURVE('',#816,#816,#730,.T.);
#971=EDGE_CURVE('',#816,#817,#479,.T.);
#972=EDGE_CURVE('',#817,#817,#731,.T.);
#973=EDGE_CURVE('',#818,#818,#732,.T.);
#974=EDGE_CURVE('',#818,#819,#480,.T.);
#975=EDGE_CURVE('',#819,#819,#733,.T.);
#976=EDGE_CURVE('',#820,#820,#734,.T.);
#977=EDGE_CURVE('',#820,#821,#481,.T.);
#978=EDGE_CURVE('',#821,#821,#735,.T.);
#979=EDGE_CURVE('',#822,#822,#736,.T.);
#980=EDGE_CURVE('',#822,#823,#482,.T.);
#981=EDGE_CURVE('',#823,#823,#737,.T.);
#982=EDGE_CURVE('',#824,#824,#738,.T.);
#983=EDGE_CURVE('',#824,#825,#483,.T.);
#984=EDGE_CURVE('',#825,#825,#739,.T.);
#985=EDGE_CURVE('',#826,#826,#740,.T.);
#986=EDGE_CURVE('',#826,#827,#484,.T.);
#987=EDGE_CURVE('',#827,#827,#741,.T.);
#988=EDGE_CURVE('',#828,#828,#742,.T.);
#989=EDGE_CURVE('',#828,#829,#485,.T.);
#990=EDGE_CURVE('',#829,#829,#743,.T.);
#991=EDGE_CURVE('',#830,#830,#744,.T.);
#992=EDGE_CURVE('',#830,#831,#486,.T.);
#993=EDGE_CURVE('',#831,#831,#745,.T.);
#994=EDGE_CURVE('',#832,#832,#746,.T.);
#995=EDGE_CURVE('',#832,#833,#487,.T.);
#996=EDGE_CURVE('',#833,#833,#747,.T.);
#997=EDGE_CURVE('',#834,#834,#748,.T.);
#998=EDGE_CURVE('',#834,#835,#488,.T.);
#999=EDGE_CURVE('',#835,#835,#749,.T.);
#1000=EDGE_CURVE('',#836,#836,#750,.T.);
#1001=EDGE_CURVE('',#836,#837,#489,.T.);
#1002=EDGE_CURVE('',#837,#837,#751,.T.);
#1003=EDGE_CURVE('',#838,#838,#752,.T.);
#1004=EDGE_CURVE('',#838,#839,#490,.T.);
#1005=EDGE_CURVE('',#839,#839,#753,.T.);
#1006=EDGE_CURVE('',#840,#840,#754,.T.);
#1007=EDGE_CURVE('',#840,#841,#491,.T.);
#1008=EDGE_CURVE('',#841,#841,#755,.T.);
#1009=EDGE_CURVE('',#842,#842,#756,.T.);
#1010=EDGE_CURVE('',#842,#843,#492,.T.);
#1011=EDGE_CURVE('',#843,#843,#757,.T.);
#1012=EDGE_CURVE('',#844,#844,#758,.T.);
#1013=EDGE_CURVE('',#844,#845,#493,.T.);
#1014=EDGE_CURVE('',#845,#845,#759,.T.);
#1015=EDGE_CURVE('',#846,#846,#760,.T.);
#1016=EDGE_CURVE('',#846,#847,#494,.T.);
#1017=EDGE_CURVE('',#847,#847,#761,.T.);
#1018=EDGE_CURVE('',#848,#848,#762,.T.);
#1019=EDGE_CURVE('',#848,#849,#495,.T.);
#1020=EDGE_CURVE('',#849,#849,#763,.T.);
#1021=EDGE_CURVE('',#850,#851,#496,.T.);
#1022=EDGE_CURVE('',#851,#852,#497,.T.);
#1023=EDGE_CURVE('',#853,#852,#498,.T.);
#1024=EDGE_CURVE('',#850,#853,#499,.T.);
#1025=EDGE_CURVE('',#854,#850,#500,.T.);
#1026=EDGE_CURVE('',#855,#853,#501,.T.);
#1027=EDGE_CURVE('',#854,#855,#502,.T.);
#1028=EDGE_CURVE('',#856,#854,#503,.T.);
#1029=EDGE_CURVE('',#857,#855,#504,.T.);
#1030=EDGE_CURVE('',#856,#857,#505,.T.);
#1031=EDGE_CURVE('',#851,#856,#506,.T.);
#1032=EDGE_CURVE('',#852,#857,#507,.T.);
#1033=EDGE_CURVE('',#858,#858,#764,.T.);
#1034=EDGE_CURVE('',#858,#859,#508,.T.);
#1035=EDGE_CURVE('',#859,#859,#765,.T.);
#1036=EDGE_CURVE('',#860,#860,#766,.T.);
#1037=EDGE_CURVE('',#860,#861,#509,.T.);
#1038=EDGE_CURVE('',#861,#861,#767,.T.);
#1039=EDGE_CURVE('',#862,#862,#768,.T.);
#1040=EDGE_CURVE('',#862,#863,#510,.T.);
#1041=EDGE_CURVE('',#863,#863,#769,.T.);
#1042=EDGE_CURVE('',#864,#864,#770,.T.);
#1043=EDGE_CURVE('',#864,#865,#511,.T.);
#1044=EDGE_CURVE('',#865,#865,#771,.T.);
#1045=EDGE_CURVE('',#866,#866,#772,.T.);
#1046=EDGE_CURVE('',#866,#867,#512,.T.);
#1047=EDGE_CURVE('',#867,#867,#64,.T.);
#1048=EDGE_CURVE('',#868,#869,#513,.T.);
#1049=EDGE_CURVE('',#868,#870,#514,.T.);
#1050=EDGE_CURVE('',#871,#870,#515,.T.);
#1051=EDGE_CURVE('',#869,#871,#516,.T.);
#1052=EDGE_CURVE('',#869,#872,#517,.T.);
#1053=EDGE_CURVE('',#873,#871,#518,.T.);
#1054=EDGE_CURVE('',#872,#873,#519,.T.);
#1055=EDGE_CURVE('',#872,#874,#520,.T.);
#1056=EDGE_CURVE('',#875,#873,#521,.T.);
#1057=EDGE_CURVE('',#874,#875,#522,.T.);
#1058=EDGE_CURVE('',#874,#868,#523,.T.);
#1059=EDGE_CURVE('',#870,#875,#524,.T.);
#1060=EDGE_CURVE('',#876,#877,#525,.T.);
#1061=EDGE_CURVE('',#878,#876,#526,.T.);
#1062=EDGE_CURVE('',#879,#878,#527,.T.);
#1063=EDGE_CURVE('',#879,#877,#528,.T.);
#1064=EDGE_CURVE('',#880,#881,#529,.T.);
#1065=EDGE_CURVE('',#882,#880,#530,.T.);
#1066=EDGE_CURVE('',#883,#882,#531,.T.);
#1067=EDGE_CURVE('',#881,#883,#532,.T.);
#1068=EDGE_CURVE('',#884,#885,#533,.T.);
#1069=EDGE_CURVE('',#884,#886,#534,.T.);
#1070=EDGE_CURVE('',#887,#886,#535,.T.);
#1071=EDGE_CURVE('',#885,#887,#536,.T.);
#1072=EDGE_CURVE('',#878,#883,#773,.T.);
#1073=EDGE_CURVE('',#882,#879,#774,.T.);
#1074=EDGE_CURVE('',#877,#880,#65,.T.);
#1075=EDGE_CURVE('',#881,#876,#66,.T.);
#1076=EDGE_CURVE('',#885,#888,#537,.T.);
#1077=EDGE_CURVE('',#889,#887,#538,.T.);
#1078=EDGE_CURVE('',#888,#889,#539,.T.);
#1079=EDGE_CURVE('',#888,#890,#540,.T.);
#1080=EDGE_CURVE('',#891,#889,#541,.T.);
#1081=EDGE_CURVE('',#890,#891,#542,.T.);
#1082=EDGE_CURVE('',#890,#884,#543,.T.);
#1083=EDGE_CURVE('',#886,#891,#544,.T.);
#1084=EDGE_CURVE('',#892,#893,#545,.T.);
#1085=EDGE_CURVE('',#893,#894,#546,.T.);
#1086=EDGE_CURVE('',#894,#895,#547,.T.);
#1087=EDGE_CURVE('',#892,#895,#548,.T.);
#1088=EDGE_CURVE('',#893,#896,#549,.T.);
#1089=EDGE_CURVE('',#896,#897,#550,.T.);
#1090=EDGE_CURVE('',#897,#894,#551,.T.);
#1091=EDGE_CURVE('',#896,#898,#552,.T.);
#1092=EDGE_CURVE('',#898,#899,#553,.T.);
#1093=EDGE_CURVE('',#899,#897,#554,.T.);
#1094=EDGE_CURVE('',#898,#900,#555,.T.);
#1095=EDGE_CURVE('',#900,#901,#556,.T.);
#1096=EDGE_CURVE('',#901,#899,#557,.T.);
#1097=EDGE_CURVE('',#900,#902,#558,.T.);
#1098=EDGE_CURVE('',#902,#903,#559,.T.);
#1099=EDGE_CURVE('',#903,#901,#560,.T.);
#1100=EDGE_CURVE('',#902,#892,#561,.T.);
#1101=EDGE_CURVE('',#895,#903,#562,.T.);
#1102=EDGE_CURVE('',#904,#904,#775,.T.);
#1103=EDGE_CURVE('',#905,#905,#776,.T.);
#1104=EDGE_CURVE('',#906,#906,#777,.T.);
#1105=EDGE_CURVE('',#906,#905,#563,.T.);
#1106=EDGE_CURVE('',#907,#907,#778,.T.);
#1107=EDGE_CURVE('',#907,#906,#564,.T.);
#1108=EDGE_CURVE('',#908,#908,#779,.T.);
#1109=EDGE_CURVE('',#908,#907,#565,.T.);
#1110=EDGE_CURVE('',#909,#909,#780,.T.);
#1111=EDGE_CURVE('',#910,#910,#781,.F.);
#1112=EDGE_CURVE('',#910,#909,#566,.T.);
#1113=EDGE_CURVE('',#904,#910,#567,.T.);
#1114=EDGE_CURVE('',#911,#911,#782,.T.);
#1115=EDGE_CURVE('',#911,#912,#568,.T.);
#1116=EDGE_CURVE('',#912,#912,#783,.T.);
#1117=EDGE_CURVE('',#913,#913,#784,.T.);
#1118=EDGE_CURVE('',#913,#914,#569,.T.);
#1119=EDGE_CURVE('',#914,#914,#785,.T.);
#1120=EDGE_CURVE('',#915,#915,#786,.F.);
#1121=EDGE_CURVE('',#915,#916,#570,.T.);
#1122=EDGE_CURVE('',#916,#916,#787,.F.);
#1123=EDGE_CURVE('',#917,#917,#788,.T.);
#1124=EDGE_CURVE('',#917,#915,#571,.T.);
#1125=EDGE_CURVE('',#918,#918,#789,.T.);
#1126=EDGE_CURVE('',#918,#919,#572,.T.);
#1127=EDGE_CURVE('',#920,#919,#51,.T.);
#1128=EDGE_CURVE('',#921,#920,#52,.T.);
#1129=EDGE_CURVE('',#922,#921,#53,.T.);
#1130=EDGE_CURVE('',#923,#922,#54,.T.);
#1131=EDGE_CURVE('',#924,#923,#55,.T.);
#1132=EDGE_CURVE('',#919,#924,#56,.T.);
#1133=EDGE_CURVE('',#925,#923,#573,.T.);
#1134=EDGE_CURVE('',#925,#926,#574,.T.);
#1135=EDGE_CURVE('',#926,#924,#575,.T.);
#1136=EDGE_CURVE('',#927,#922,#576,.T.);
#1137=EDGE_CURVE('',#927,#925,#577,.T.);
#1138=EDGE_CURVE('',#928,#921,#578,.T.);
#1139=EDGE_CURVE('',#928,#927,#579,.T.);
#1140=EDGE_CURVE('',#929,#920,#580,.T.);
#1141=EDGE_CURVE('',#929,#928,#581,.T.);
#1142=EDGE_CURVE('',#930,#919,#582,.T.);
#1143=EDGE_CURVE('',#930,#929,#583,.T.);
#1144=EDGE_CURVE('',#926,#930,#584,.T.);
#1145=ORIENTED_EDGE('',*,*,#931,.F.);
#1146=ORIENTED_EDGE('',*,*,#932,.T.);
#1147=ORIENTED_EDGE('',*,*,#933,.F.);
#1148=ORIENTED_EDGE('',*,*,#932,.F.);
#1149=ORIENTED_EDGE('',*,*,#934,.F.);
#1150=ORIENTED_EDGE('',*,*,#935,.T.);
#1151=ORIENTED_EDGE('',*,*,#936,.F.);
#1152=ORIENTED_EDGE('',*,*,#935,.F.);
#1153=ORIENTED_EDGE('',*,*,#937,.F.);
#1154=ORIENTED_EDGE('',*,*,#938,.T.);
#1155=ORIENTED_EDGE('',*,*,#939,.F.);
#1156=ORIENTED_EDGE('',*,*,#938,.F.);
#1157=ORIENTED_EDGE('',*,*,#940,.F.);
#1158=ORIENTED_EDGE('',*,*,#941,.T.);
#1159=ORIENTED_EDGE('',*,*,#942,.F.);
#1160=ORIENTED_EDGE('',*,*,#941,.F.);
#1161=ORIENTED_EDGE('',*,*,#943,.F.);
#1162=ORIENTED_EDGE('',*,*,#944,.T.);
#1163=ORIENTED_EDGE('',*,*,#945,.F.);
#1164=ORIENTED_EDGE('',*,*,#944,.F.);
#1165=ORIENTED_EDGE('',*,*,#946,.F.);
#1166=ORIENTED_EDGE('',*,*,#947,.T.);
#1167=ORIENTED_EDGE('',*,*,#948,.F.);
#1168=ORIENTED_EDGE('',*,*,#947,.F.);
#1169=ORIENTED_EDGE('',*,*,#949,.F.);
#1170=ORIENTED_EDGE('',*,*,#950,.T.);
#1171=ORIENTED_EDGE('',*,*,#951,.F.);
#1172=ORIENTED_EDGE('',*,*,#950,.F.);
#1173=ORIENTED_EDGE('',*,*,#952,.F.);
#1174=ORIENTED_EDGE('',*,*,#953,.T.);
#1175=ORIENTED_EDGE('',*,*,#954,.F.);
#1176=ORIENTED_EDGE('',*,*,#953,.F.);
#1177=ORIENTED_EDGE('',*,*,#955,.F.);
#1178=ORIENTED_EDGE('',*,*,#956,.T.);
#1179=ORIENTED_EDGE('',*,*,#957,.F.);
#1180=ORIENTED_EDGE('',*,*,#956,.F.);
#1181=ORIENTED_EDGE('',*,*,#958,.F.);
#1182=ORIENTED_EDGE('',*,*,#959,.T.);
#1183=ORIENTED_EDGE('',*,*,#960,.F.);
#1184=ORIENTED_EDGE('',*,*,#959,.F.);
#1185=ORIENTED_EDGE('',*,*,#961,.F.);
#1186=ORIENTED_EDGE('',*,*,#962,.T.);
#1187=ORIENTED_EDGE('',*,*,#963,.F.);
#1188=ORIENTED_EDGE('',*,*,#962,.F.);
#1189=ORIENTED_EDGE('',*,*,#964,.F.);
#1190=ORIENTED_EDGE('',*,*,#965,.T.);
#1191=ORIENTED_EDGE('',*,*,#966,.F.);
#1192=ORIENTED_EDGE('',*,*,#965,.F.);
#1193=ORIENTED_EDGE('',*,*,#967,.F.);
#1194=ORIENTED_EDGE('',*,*,#968,.T.);
#1195=ORIENTED_EDGE('',*,*,#969,.F.);
#1196=ORIENTED_EDGE('',*,*,#968,.F.);
#1197=ORIENTED_EDGE('',*,*,#970,.F.);
#1198=ORIENTED_EDGE('',*,*,#971,.T.);
#1199=ORIENTED_EDGE('',*,*,#972,.F.);
#1200=ORIENTED_EDGE('',*,*,#971,.F.);
#1201=ORIENTED_EDGE('',*,*,#973,.F.);
#1202=ORIENTED_EDGE('',*,*,#974,.T.);
#1203=ORIENTED_EDGE('',*,*,#975,.F.);
#1204=ORIENTED_EDGE('',*,*,#974,.F.);
#1205=ORIENTED_EDGE('',*,*,#976,.F.);
#1206=ORIENTED_EDGE('',*,*,#977,.T.);
#1207=ORIENTED_EDGE('',*,*,#978,.F.);
#1208=ORIENTED_EDGE('',*,*,#977,.F.);
#1209=ORIENTED_EDGE('',*,*,#979,.F.);
#1210=ORIENTED_EDGE('',*,*,#980,.T.);
#1211=ORIENTED_EDGE('',*,*,#981,.F.);
#1212=ORIENTED_EDGE('',*,*,#980,.F.);
#1213=ORIENTED_EDGE('',*,*,#982,.F.);
#1214=ORIENTED_EDGE('',*,*,#983,.T.);
#1215=ORIENTED_EDGE('',*,*,#984,.F.);
#1216=ORIENTED_EDGE('',*,*,#983,.F.);
#1217=ORIENTED_EDGE('',*,*,#985,.F.);
#1218=ORIENTED_EDGE('',*,*,#986,.T.);
#1219=ORIENTED_EDGE('',*,*,#987,.F.);
#1220=ORIENTED_EDGE('',*,*,#986,.F.);
#1221=ORIENTED_EDGE('',*,*,#988,.F.);
#1222=ORIENTED_EDGE('',*,*,#989,.T.);
#1223=ORIENTED_EDGE('',*,*,#990,.F.);
#1224=ORIENTED_EDGE('',*,*,#989,.F.);
#1225=ORIENTED_EDGE('',*,*,#991,.F.);
#1226=ORIENTED_EDGE('',*,*,#992,.T.);
#1227=ORIENTED_EDGE('',*,*,#993,.F.);
#1228=ORIENTED_EDGE('',*,*,#992,.F.);
#1229=ORIENTED_EDGE('',*,*,#994,.F.);
#1230=ORIENTED_EDGE('',*,*,#995,.T.);
#1231=ORIENTED_EDGE('',*,*,#996,.F.);
#1232=ORIENTED_EDGE('',*,*,#995,.F.);
#1233=ORIENTED_EDGE('',*,*,#997,.F.);
#1234=ORIENTED_EDGE('',*,*,#998,.T.);
#1235=ORIENTED_EDGE('',*,*,#999,.F.);
#1236=ORIENTED_EDGE('',*,*,#998,.F.);
#1237=ORIENTED_EDGE('',*,*,#1000,.F.);
#1238=ORIENTED_EDGE('',*,*,#1001,.T.);
#1239=ORIENTED_EDGE('',*,*,#1002,.F.);
#1240=ORIENTED_EDGE('',*,*,#1001,.F.);
#1241=ORIENTED_EDGE('',*,*,#1003,.F.);
#1242=ORIENTED_EDGE('',*,*,#1004,.T.);
#1243=ORIENTED_EDGE('',*,*,#1005,.F.);
#1244=ORIENTED_EDGE('',*,*,#1004,.F.);
#1245=ORIENTED_EDGE('',*,*,#1006,.F.);
#1246=ORIENTED_EDGE('',*,*,#1007,.T.);
#1247=ORIENTED_EDGE('',*,*,#1008,.F.);
#1248=ORIENTED_EDGE('',*,*,#1007,.F.);
#1249=ORIENTED_EDGE('',*,*,#1009,.F.);
#1250=ORIENTED_EDGE('',*,*,#1010,.T.);
#1251=ORIENTED_EDGE('',*,*,#1011,.F.);
#1252=ORIENTED_EDGE('',*,*,#1010,.F.);
#1253=ORIENTED_EDGE('',*,*,#1012,.F.);
#1254=ORIENTED_EDGE('',*,*,#1013,.T.);
#1255=ORIENTED_EDGE('',*,*,#1014,.F.);
#1256=ORIENTED_EDGE('',*,*,#1013,.F.);
#1257=ORIENTED_EDGE('',*,*,#1015,.F.);
#1258=ORIENTED_EDGE('',*,*,#1016,.T.);
#1259=ORIENTED_EDGE('',*,*,#1017,.F.);
#1260=ORIENTED_EDGE('',*,*,#1016,.F.);
#1261=ORIENTED_EDGE('',*,*,#1018,.F.);
#1262=ORIENTED_EDGE('',*,*,#1019,.T.);
#1263=ORIENTED_EDGE('',*,*,#1020,.F.);
#1264=ORIENTED_EDGE('',*,*,#1019,.F.);
#1265=ORIENTED_EDGE('',*,*,#1021,.T.);
#1266=ORIENTED_EDGE('',*,*,#1022,.T.);
#1267=ORIENTED_EDGE('',*,*,#1023,.F.);
#1268=ORIENTED_EDGE('',*,*,#1024,.F.);
#1269=ORIENTED_EDGE('',*,*,#1025,.T.);
#1270=ORIENTED_EDGE('',*,*,#1024,.T.);
#1271=ORIENTED_EDGE('',*,*,#1026,.F.);
#1272=ORIENTED_EDGE('',*,*,#1027,.F.);
#1273=ORIENTED_EDGE('',*,*,#1028,.T.);
#1274=ORIENTED_EDGE('',*,*,#1027,.T.);
#1275=ORIENTED_EDGE('',*,*,#1029,.F.);
#1276=ORIENTED_EDGE('',*,*,#1030,.F.);
#1277=ORIENTED_EDGE('',*,*,#1031,.T.);
#1278=ORIENTED_EDGE('',*,*,#1030,.T.);
#1279=ORIENTED_EDGE('',*,*,#1032,.F.);
#1280=ORIENTED_EDGE('',*,*,#1022,.F.);
#1281=ORIENTED_EDGE('',*,*,#1032,.T.);
#1282=ORIENTED_EDGE('',*,*,#1029,.T.);
#1283=ORIENTED_EDGE('',*,*,#1026,.T.);
#1284=ORIENTED_EDGE('',*,*,#1023,.T.);
#1285=ORIENTED_EDGE('',*,*,#945,.T.);
#1286=ORIENTED_EDGE('',*,*,#1020,.T.);
#1287=ORIENTED_EDGE('',*,*,#1017,.T.);
#1288=ORIENTED_EDGE('',*,*,#1014,.T.);
#1289=ORIENTED_EDGE('',*,*,#1011,.T.);
#1290=ORIENTED_EDGE('',*,*,#1008,.T.);
#1291=ORIENTED_EDGE('',*,*,#1005,.T.);
#1292=ORIENTED_EDGE('',*,*,#1002,.T.);
#1293=ORIENTED_EDGE('',*,*,#999,.T.);
#1294=ORIENTED_EDGE('',*,*,#996,.T.);
#1295=ORIENTED_EDGE('',*,*,#993,.T.);
#1296=ORIENTED_EDGE('',*,*,#990,.T.);
#1297=ORIENTED_EDGE('',*,*,#987,.T.);
#1298=ORIENTED_EDGE('',*,*,#984,.T.);
#1299=ORIENTED_EDGE('',*,*,#981,.T.);
#1300=ORIENTED_EDGE('',*,*,#978,.T.);
#1301=ORIENTED_EDGE('',*,*,#975,.T.);
#1302=ORIENTED_EDGE('',*,*,#972,.T.);
#1303=ORIENTED_EDGE('',*,*,#969,.T.);
#1304=ORIENTED_EDGE('',*,*,#966,.T.);
#1305=ORIENTED_EDGE('',*,*,#963,.T.);
#1306=ORIENTED_EDGE('',*,*,#960,.T.);
#1307=ORIENTED_EDGE('',*,*,#957,.T.);
#1308=ORIENTED_EDGE('',*,*,#954,.T.);
#1309=ORIENTED_EDGE('',*,*,#951,.T.);
#1310=ORIENTED_EDGE('',*,*,#948,.T.);
#1311=ORIENTED_EDGE('',*,*,#942,.T.);
#1312=ORIENTED_EDGE('',*,*,#939,.T.);
#1313=ORIENTED_EDGE('',*,*,#936,.T.);
#1314=ORIENTED_EDGE('',*,*,#933,.T.);
#1315=ORIENTED_EDGE('',*,*,#1031,.F.);
#1316=ORIENTED_EDGE('',*,*,#1021,.F.);
#1317=ORIENTED_EDGE('',*,*,#1025,.F.);
#1318=ORIENTED_EDGE('',*,*,#1028,.F.);
#1319=ORIENTED_EDGE('',*,*,#943,.T.);
#1320=ORIENTED_EDGE('',*,*,#1018,.T.);
#1321=ORIENTED_EDGE('',*,*,#1015,.T.);
#1322=ORIENTED_EDGE('',*,*,#1012,.T.);
#1323=ORIENTED_EDGE('',*,*,#1009,.T.);
#1324=ORIENTED_EDGE('',*,*,#1006,.T.);
#1325=ORIENTED_EDGE('',*,*,#1003,.T.);
#1326=ORIENTED_EDGE('',*,*,#1000,.T.);
#1327=ORIENTED_EDGE('',*,*,#997,.T.);
#1328=ORIENTED_EDGE('',*,*,#994,.T.);
#1329=ORIENTED_EDGE('',*,*,#991,.T.);
#1330=ORIENTED_EDGE('',*,*,#988,.T.);
#1331=ORIENTED_EDGE('',*,*,#985,.T.);
#1332=ORIENTED_EDGE('',*,*,#982,.T.);
#1333=ORIENTED_EDGE('',*,*,#979,.T.);
#1334=ORIENTED_EDGE('',*,*,#976,.T.);
#1335=ORIENTED_EDGE('',*,*,#973,.T.);
#1336=ORIENTED_EDGE('',*,*,#970,.T.);
#1337=ORIENTED_EDGE('',*,*,#967,.T.);
#1338=ORIENTED_EDGE('',*,*,#964,.T.);
#1339=ORIENTED_EDGE('',*,*,#961,.T.);
#1340=ORIENTED_EDGE('',*,*,#958,.T.);
#1341=ORIENTED_EDGE('',*,*,#955,.T.);
#1342=ORIENTED_EDGE('',*,*,#952,.T.);
#1343=ORIENTED_EDGE('',*,*,#949,.T.);
#1344=ORIENTED_EDGE('',*,*,#946,.T.);
#1345=ORIENTED_EDGE('',*,*,#940,.T.);
#1346=ORIENTED_EDGE('',*,*,#937,.T.);
#1347=ORIENTED_EDGE('',*,*,#934,.T.);
#1348=ORIENTED_EDGE('',*,*,#931,.T.);
#1349=ORIENTED_EDGE('',*,*,#1033,.F.);
#1350=ORIENTED_EDGE('',*,*,#1034,.T.);
#1351=ORIENTED_EDGE('',*,*,#1035,.T.);
#1352=ORIENTED_EDGE('',*,*,#1034,.F.);
#1353=ORIENTED_EDGE('',*,*,#1035,.F.);
#1354=ORIENTED_EDGE('',*,*,#1036,.F.);
#1355=ORIENTED_EDGE('',*,*,#1037,.T.);
#1356=ORIENTED_EDGE('',*,*,#1038,.T.);
#1357=ORIENTED_EDGE('',*,*,#1037,.F.);
#1358=ORIENTED_EDGE('',*,*,#1038,.F.);
#1359=ORIENTED_EDGE('',*,*,#1039,.F.);
#1360=ORIENTED_EDGE('',*,*,#1040,.T.);
#1361=ORIENTED_EDGE('',*,*,#1041,.T.);
#1362=ORIENTED_EDGE('',*,*,#1040,.F.);
#1363=ORIENTED_EDGE('',*,*,#1041,.F.);
#1364=ORIENTED_EDGE('',*,*,#1042,.F.);
#1365=ORIENTED_EDGE('',*,*,#1043,.T.);
#1366=ORIENTED_EDGE('',*,*,#1044,.T.);
#1367=ORIENTED_EDGE('',*,*,#1043,.F.);
#1368=ORIENTED_EDGE('',*,*,#1044,.F.);
#1369=ORIENTED_EDGE('',*,*,#1045,.F.);
#1370=ORIENTED_EDGE('',*,*,#1046,.T.);
#1371=ORIENTED_EDGE('',*,*,#1047,.F.);
#1372=ORIENTED_EDGE('',*,*,#1046,.F.);
#1373=ORIENTED_EDGE('',*,*,#1048,.F.);
#1374=ORIENTED_EDGE('',*,*,#1049,.T.);
#1375=ORIENTED_EDGE('',*,*,#1050,.F.);
#1376=ORIENTED_EDGE('',*,*,#1051,.F.);
#1377=ORIENTED_EDGE('',*,*,#1052,.F.);
#1378=ORIENTED_EDGE('',*,*,#1051,.T.);
#1379=ORIENTED_EDGE('',*,*,#1053,.F.);
#1380=ORIENTED_EDGE('',*,*,#1054,.F.);
#1381=ORIENTED_EDGE('',*,*,#1045,.T.);
#1382=ORIENTED_EDGE('',*,*,#1042,.T.);
#1383=ORIENTED_EDGE('',*,*,#1039,.T.);
#1384=ORIENTED_EDGE('',*,*,#1036,.T.);
#1385=ORIENTED_EDGE('',*,*,#1033,.T.);
#1386=ORIENTED_EDGE('',*,*,#1055,.F.);
#1387=ORIENTED_EDGE('',*,*,#1054,.T.);
#1388=ORIENTED_EDGE('',*,*,#1056,.F.);
#1389=ORIENTED_EDGE('',*,*,#1057,.F.);
#1390=ORIENTED_EDGE('',*,*,#1058,.F.);
#1391=ORIENTED_EDGE('',*,*,#1057,.T.);
#1392=ORIENTED_EDGE('',*,*,#1059,.F.);
#1393=ORIENTED_EDGE('',*,*,#1049,.F.);
#1394=ORIENTED_EDGE('',*,*,#1047,.T.);
#1395=ORIENTED_EDGE('',*,*,#1059,.T.);
#1396=ORIENTED_EDGE('',*,*,#1056,.T.);
#1397=ORIENTED_EDGE('',*,*,#1053,.T.);
#1398=ORIENTED_EDGE('',*,*,#1050,.T.);
#1399=ORIENTED_EDGE('',*,*,#1058,.T.);
#1400=ORIENTED_EDGE('',*,*,#1048,.T.);
#1401=ORIENTED_EDGE('',*,*,#1052,.T.);
#1402=ORIENTED_EDGE('',*,*,#1055,.T.);
#1403=ORIENTED_EDGE('',*,*,#1060,.F.);
#1404=ORIENTED_EDGE('',*,*,#1061,.F.);
#1405=ORIENTED_EDGE('',*,*,#1062,.F.);
#1406=ORIENTED_EDGE('',*,*,#1063,.T.);
#1407=ORIENTED_EDGE('',*,*,#1064,.F.);
#1408=ORIENTED_EDGE('',*,*,#1065,.F.);
#1409=ORIENTED_EDGE('',*,*,#1066,.F.);
#1410=ORIENTED_EDGE('',*,*,#1067,.F.);
#1411=ORIENTED_EDGE('',*,*,#1068,.F.);
#1412=ORIENTED_EDGE('',*,*,#1069,.T.);
#1413=ORIENTED_EDGE('',*,*,#1070,.F.);
#1414=ORIENTED_EDGE('',*,*,#1071,.F.);
#1415=ORIENTED_EDGE('',*,*,#1062,.T.);
#1416=ORIENTED_EDGE('',*,*,#1072,.T.);
#1417=ORIENTED_EDGE('',*,*,#1066,.T.);
#1418=ORIENTED_EDGE('',*,*,#1073,.T.);
#1419=ORIENTED_EDGE('',*,*,#1063,.F.);
#1420=ORIENTED_EDGE('',*,*,#1073,.F.);
#1421=ORIENTED_EDGE('',*,*,#1065,.T.);
#1422=ORIENTED_EDGE('',*,*,#1074,.F.);
#1423=ORIENTED_EDGE('',*,*,#1061,.T.);
#1424=ORIENTED_EDGE('',*,*,#1075,.F.);
#1425=ORIENTED_EDGE('',*,*,#1067,.T.);
#1426=ORIENTED_EDGE('',*,*,#1072,.F.);
#1427=ORIENTED_EDGE('',*,*,#1076,.F.);
#1428=ORIENTED_EDGE('',*,*,#1071,.T.);
#1429=ORIENTED_EDGE('',*,*,#1077,.F.);
#1430=ORIENTED_EDGE('',*,*,#1078,.F.);
#1431=ORIENTED_EDGE('',*,*,#1079,.F.);
#1432=ORIENTED_EDGE('',*,*,#1078,.T.);
#1433=ORIENTED_EDGE('',*,*,#1080,.F.);
#1434=ORIENTED_EDGE('',*,*,#1081,.F.);
#1435=ORIENTED_EDGE('',*,*,#1060,.T.);
#1436=ORIENTED_EDGE('',*,*,#1074,.T.);
#1437=ORIENTED_EDGE('',*,*,#1064,.T.);
#1438=ORIENTED_EDGE('',*,*,#1075,.T.);
#1439=ORIENTED_EDGE('',*,*,#1082,.F.);
#1440=ORIENTED_EDGE('',*,*,#1081,.T.);
#1441=ORIENTED_EDGE('',*,*,#1083,.F.);
#1442=ORIENTED_EDGE('',*,*,#1069,.F.);
#1443=ORIENTED_EDGE('',*,*,#1070,.T.);
#1444=ORIENTED_EDGE('',*,*,#1083,.T.);
#1445=ORIENTED_EDGE('',*,*,#1080,.T.);
#1446=ORIENTED_EDGE('',*,*,#1077,.T.);
#1447=ORIENTED_EDGE('',*,*,#1068,.T.);
#1448=ORIENTED_EDGE('',*,*,#1076,.T.);
#1449=ORIENTED_EDGE('',*,*,#1079,.T.);
#1450=ORIENTED_EDGE('',*,*,#1082,.T.);
#1451=ORIENTED_EDGE('',*,*,#1084,.T.);
#1452=ORIENTED_EDGE('',*,*,#1085,.T.);
#1453=ORIENTED_EDGE('',*,*,#1086,.T.);
#1454=ORIENTED_EDGE('',*,*,#1087,.F.);
#1455=ORIENTED_EDGE('',*,*,#1088,.T.);
#1456=ORIENTED_EDGE('',*,*,#1089,.T.);
#1457=ORIENTED_EDGE('',*,*,#1090,.T.);
#1458=ORIENTED_EDGE('',*,*,#1085,.F.);
#1459=ORIENTED_EDGE('',*,*,#1091,.T.);
#1460=ORIENTED_EDGE('',*,*,#1092,.T.);
#1461=ORIENTED_EDGE('',*,*,#1093,.T.);
#1462=ORIENTED_EDGE('',*,*,#1089,.F.);
#1463=ORIENTED_EDGE('',*,*,#1094,.T.);
#1464=ORIENTED_EDGE('',*,*,#1095,.T.);
#1465=ORIENTED_EDGE('',*,*,#1096,.T.);
#1466=ORIENTED_EDGE('',*,*,#1092,.F.);
#1467=ORIENTED_EDGE('',*,*,#1097,.T.);
#1468=ORIENTED_EDGE('',*,*,#1098,.T.);
#1469=ORIENTED_EDGE('',*,*,#1099,.T.);
#1470=ORIENTED_EDGE('',*,*,#1095,.F.);
#1471=ORIENTED_EDGE('',*,*,#1100,.T.);
#1472=ORIENTED_EDGE('',*,*,#1087,.T.);
#1473=ORIENTED_EDGE('',*,*,#1101,.T.);
#1474=ORIENTED_EDGE('',*,*,#1098,.F.);
#1475=ORIENTED_EDGE('',*,*,#1100,.F.);
#1476=ORIENTED_EDGE('',*,*,#1097,.F.);
#1477=ORIENTED_EDGE('',*,*,#1094,.F.);
#1478=ORIENTED_EDGE('',*,*,#1091,.F.);
#1479=ORIENTED_EDGE('',*,*,#1088,.F.);
#1480=ORIENTED_EDGE('',*,*,#1084,.F.);
#1481=ORIENTED_EDGE('',*,*,#1101,.F.);
#1482=ORIENTED_EDGE('',*,*,#1086,.F.);
#1483=ORIENTED_EDGE('',*,*,#1090,.F.);
#1484=ORIENTED_EDGE('',*,*,#1093,.F.);
#1485=ORIENTED_EDGE('',*,*,#1096,.F.);
#1486=ORIENTED_EDGE('',*,*,#1099,.F.);
#1487=ORIENTED_EDGE('',*,*,#1102,.F.);
#1488=ORIENTED_EDGE('',*,*,#1103,.F.);
#1489=ORIENTED_EDGE('',*,*,#1104,.F.);
#1490=ORIENTED_EDGE('',*,*,#1105,.T.);
#1491=ORIENTED_EDGE('',*,*,#1103,.T.);
#1492=ORIENTED_EDGE('',*,*,#1105,.F.);
#1493=ORIENTED_EDGE('',*,*,#1106,.F.);
#1494=ORIENTED_EDGE('',*,*,#1107,.T.);
#1495=ORIENTED_EDGE('',*,*,#1104,.T.);
#1496=ORIENTED_EDGE('',*,*,#1107,.F.);
#1497=ORIENTED_EDGE('',*,*,#1108,.F.);
#1498=ORIENTED_EDGE('',*,*,#1109,.T.);
#1499=ORIENTED_EDGE('',*,*,#1106,.T.);
#1500=ORIENTED_EDGE('',*,*,#1109,.F.);
#1501=ORIENTED_EDGE('',*,*,#1108,.T.);
#1502=ORIENTED_EDGE('',*,*,#1110,.F.);
#1503=ORIENTED_EDGE('',*,*,#1111,.F.);
#1504=ORIENTED_EDGE('',*,*,#1112,.T.);
#1505=ORIENTED_EDGE('',*,*,#1110,.T.);
#1506=ORIENTED_EDGE('',*,*,#1112,.F.);
#1507=ORIENTED_EDGE('',*,*,#1102,.T.);
#1508=ORIENTED_EDGE('',*,*,#1113,.T.);
#1509=ORIENTED_EDGE('',*,*,#1111,.T.);
#1510=ORIENTED_EDGE('',*,*,#1113,.F.);
#1511=ORIENTED_EDGE('',*,*,#1114,.F.);
#1512=ORIENTED_EDGE('',*,*,#1115,.T.);
#1513=ORIENTED_EDGE('',*,*,#1116,.T.);
#1514=ORIENTED_EDGE('',*,*,#1115,.F.);
#1515=ORIENTED_EDGE('',*,*,#1117,.F.);
#1516=ORIENTED_EDGE('',*,*,#1118,.T.);
#1517=ORIENTED_EDGE('',*,*,#1119,.T.);
#1518=ORIENTED_EDGE('',*,*,#1118,.F.);
#1519=ORIENTED_EDGE('',*,*,#1117,.T.);
#1520=ORIENTED_EDGE('',*,*,#1114,.T.);
#1521=ORIENTED_EDGE('',*,*,#1119,.F.);
#1522=ORIENTED_EDGE('',*,*,#1116,.F.);
#1523=ORIENTED_EDGE('',*,*,#1120,.F.);
#1524=ORIENTED_EDGE('',*,*,#1121,.T.);
#1525=ORIENTED_EDGE('',*,*,#1122,.F.);
#1526=ORIENTED_EDGE('',*,*,#1121,.F.);
#1527=ORIENTED_EDGE('',*,*,#1123,.F.);
#1528=ORIENTED_EDGE('',*,*,#1124,.T.);
#1529=ORIENTED_EDGE('',*,*,#1120,.T.);
#1530=ORIENTED_EDGE('',*,*,#1124,.F.);
#1531=ORIENTED_EDGE('',*,*,#1123,.T.);
#1532=ORIENTED_EDGE('',*,*,#1125,.F.);
#1533=ORIENTED_EDGE('',*,*,#1126,.T.);
#1534=ORIENTED_EDGE('',*,*,#1127,.F.);
#1535=ORIENTED_EDGE('',*,*,#1128,.F.);
#1536=ORIENTED_EDGE('',*,*,#1129,.F.);
#1537=ORIENTED_EDGE('',*,*,#1130,.F.);
#1538=ORIENTED_EDGE('',*,*,#1131,.F.);
#1539=ORIENTED_EDGE('',*,*,#1132,.F.);
#1540=ORIENTED_EDGE('',*,*,#1126,.F.);
#1541=ORIENTED_EDGE('',*,*,#1131,.T.);
#1542=ORIENTED_EDGE('',*,*,#1133,.F.);
#1543=ORIENTED_EDGE('',*,*,#1134,.T.);
#1544=ORIENTED_EDGE('',*,*,#1135,.T.);
#1545=ORIENTED_EDGE('',*,*,#1130,.T.);
#1546=ORIENTED_EDGE('',*,*,#1136,.F.);
#1547=ORIENTED_EDGE('',*,*,#1137,.T.);
#1548=ORIENTED_EDGE('',*,*,#1133,.T.);
#1549=ORIENTED_EDGE('',*,*,#1129,.T.);
#1550=ORIENTED_EDGE('',*,*,#1138,.F.);
#1551=ORIENTED_EDGE('',*,*,#1139,.T.);
#1552=ORIENTED_EDGE('',*,*,#1136,.T.);
#1553=ORIENTED_EDGE('',*,*,#1128,.T.);
#1554=ORIENTED_EDGE('',*,*,#1140,.F.);
#1555=ORIENTED_EDGE('',*,*,#1141,.T.);
#1556=ORIENTED_EDGE('',*,*,#1138,.T.);
#1557=ORIENTED_EDGE('',*,*,#1127,.T.);
#1558=ORIENTED_EDGE('',*,*,#1142,.F.);
#1559=ORIENTED_EDGE('',*,*,#1143,.T.);
#1560=ORIENTED_EDGE('',*,*,#1140,.T.);
#1561=ORIENTED_EDGE('',*,*,#1132,.T.);
#1562=ORIENTED_EDGE('',*,*,#1135,.F.);
#1563=ORIENTED_EDGE('',*,*,#1144,.T.);
#1564=ORIENTED_EDGE('',*,*,#1142,.T.);
#1565=ORIENTED_EDGE('',*,*,#1125,.T.);
#1566=ORIENTED_EDGE('',*,*,#1139,.F.);
#1567=ORIENTED_EDGE('',*,*,#1141,.F.);
#1568=ORIENTED_EDGE('',*,*,#1143,.F.);
#1569=ORIENTED_EDGE('',*,*,#1144,.F.);
#1570=ORIENTED_EDGE('',*,*,#1134,.F.);
#1571=ORIENTED_EDGE('',*,*,#1137,.F.);
#1572=ORIENTED_EDGE('',*,*,#1122,.T.);
#1573=CYLINDRICAL_SURFACE('',#1785,0.275);
#1574=CYLINDRICAL_SURFACE('',#1788,0.275);
#1575=CYLINDRICAL_SURFACE('',#1791,0.275);
#1576=CYLINDRICAL_SURFACE('',#1794,0.275);
#1577=CYLINDRICAL_SURFACE('',#1797,0.34);
#1578=CYLINDRICAL_SURFACE('',#1800,0.34);
#1579=CYLINDRICAL_SURFACE('',#1803,0.34);
#1580=CYLINDRICAL_SURFACE('',#1806,0.34);
#1581=CYLINDRICAL_SURFACE('',#1809,0.34);
#1582=CYLINDRICAL_SURFACE('',#1812,0.34);
#1583=CYLINDRICAL_SURFACE('',#1815,0.34);
#1584=CYLINDRICAL_SURFACE('',#1818,0.34);
#1585=CYLINDRICAL_SURFACE('',#1821,0.34);
#1586=CYLINDRICAL_SURFACE('',#1824,0.34);
#1587=CYLINDRICAL_SURFACE('',#1827,0.34);
#1588=CYLINDRICAL_SURFACE('',#1830,0.34);
#1589=CYLINDRICAL_SURFACE('',#1833,0.34);
#1590=CYLINDRICAL_SURFACE('',#1836,0.34);
#1591=CYLINDRICAL_SURFACE('',#1839,0.34);
#1592=CYLINDRICAL_SURFACE('',#1842,0.34);
#1593=CYLINDRICAL_SURFACE('',#1845,0.34);
#1594=CYLINDRICAL_SURFACE('',#1848,0.34);
#1595=CYLINDRICAL_SURFACE('',#1851,0.34);
#1596=CYLINDRICAL_SURFACE('',#1854,0.34);
#1597=CYLINDRICAL_SURFACE('',#1857,0.34);
#1598=CYLINDRICAL_SURFACE('',#1860,0.34);
#1599=CYLINDRICAL_SURFACE('',#1863,0.34);
#1600=CYLINDRICAL_SURFACE('',#1866,0.34);
#1601=CYLINDRICAL_SURFACE('',#1869,0.34);
#1602=CYLINDRICAL_SURFACE('',#1872,0.34);
#1603=CYLINDRICAL_SURFACE('',#1882,0.21);
#1604=CYLINDRICAL_SURFACE('',#1886,0.21);
#1605=CYLINDRICAL_SURFACE('',#1890,0.21);
#1606=CYLINDRICAL_SURFACE('',#1894,0.21);
#1607=CYLINDRICAL_SURFACE('',#1898,0.425);
#1608=CYLINDRICAL_SURFACE('',#1913,0.45);
#1609=CYLINDRICAL_SURFACE('',#1915,0.45);
#1610=CYLINDRICAL_SURFACE('',#1937,0.425);
#1611=CYLINDRICAL_SURFACE('',#1945,0.24505);
#1612=CYLINDRICAL_SURFACE('',#1947,0.42);
#1613=CYLINDRICAL_SURFACE('',#1950,0.8);
#1614=CYLINDRICAL_SURFACE('',#1956,0.3933);
#1615=ADVANCED_FACE('',(#208),#1573,.F.);
#1616=ADVANCED_FACE('',(#209),#1574,.F.);
#1617=ADVANCED_FACE('',(#210),#1575,.F.);
#1618=ADVANCED_FACE('',(#211),#1576,.F.);
#1619=ADVANCED_FACE('',(#212),#1577,.F.);
#1620=ADVANCED_FACE('',(#213),#1578,.F.);
#1621=ADVANCED_FACE('',(#214),#1579,.F.);
#1622=ADVANCED_FACE('',(#215),#1580,.F.);
#1623=ADVANCED_FACE('',(#216),#1581,.F.);
#1624=ADVANCED_FACE('',(#217),#1582,.F.);
#1625=ADVANCED_FACE('',(#218),#1583,.F.);
#1626=ADVANCED_FACE('',(#219),#1584,.F.);
#1627=ADVANCED_FACE('',(#220),#1585,.F.);
#1628=ADVANCED_FACE('',(#221),#1586,.F.);
#1629=ADVANCED_FACE('',(#222),#1587,.F.);
#1630=ADVANCED_FACE('',(#223),#1588,.F.);
#1631=ADVANCED_FACE('',(#224),#1589,.F.);
#1632=ADVANCED_FACE('',(#225),#1590,.F.);
#1633=ADVANCED_FACE('',(#226),#1591,.F.);
#1634=ADVANCED_FACE('',(#227),#1592,.F.);
#1635=ADVANCED_FACE('',(#228),#1593,.F.);
#1636=ADVANCED_FACE('',(#229),#1594,.F.);
#1637=ADVANCED_FACE('',(#230),#1595,.F.);
#1638=ADVANCED_FACE('',(#231),#1596,.F.);
#1639=ADVANCED_FACE('',(#232),#1597,.F.);
#1640=ADVANCED_FACE('',(#233),#1598,.F.);
#1641=ADVANCED_FACE('',(#234),#1599,.F.);
#1642=ADVANCED_FACE('',(#235),#1600,.F.);
#1643=ADVANCED_FACE('',(#236),#1601,.F.);
#1644=ADVANCED_FACE('',(#237),#1602,.F.);
#1645=ADVANCED_FACE('',(#238),#162,.T.);
#1646=ADVANCED_FACE('',(#239),#163,.T.);
#1647=ADVANCED_FACE('',(#240),#164,.T.);
#1648=ADVANCED_FACE('',(#241),#165,.T.);
#1649=ADVANCED_FACE('',(#242,#90,#91,#92,#93,#94,#95,#96,#97,#98,#99,#100,
#101,#102,#103,#104,#105,#106,#107,#108,#109,#110,#111,#112,#113,#114,#115,
#116,#117,#118,#119),#166,.T.);
#1650=ADVANCED_FACE('',(#243,#120,#121,#122,#123,#124,#125,#126,#127,#128,
#129,#130,#131,#132,#133,#134,#135,#136,#137,#138,#139,#140,#141,#142,#143,
#144,#145,#146,#147,#148,#149),#167,.F.);
#1651=ADVANCED_FACE('',(#244),#1603,.F.);
#1652=ADVANCED_FACE('',(#245),#168,.F.);
#1653=ADVANCED_FACE('',(#246),#1604,.F.);
#1654=ADVANCED_FACE('',(#247),#169,.F.);
#1655=ADVANCED_FACE('',(#248),#1605,.F.);
#1656=ADVANCED_FACE('',(#249),#170,.F.);
#1657=ADVANCED_FACE('',(#250),#1606,.F.);
#1658=ADVANCED_FACE('',(#251),#171,.F.);
#1659=ADVANCED_FACE('',(#252),#1607,.F.);
#1660=ADVANCED_FACE('',(#253),#172,.T.);
#1661=ADVANCED_FACE('',(#254,#150,#151,#152,#153,#154),#173,.T.);
#1662=ADVANCED_FACE('',(#255),#174,.T.);
#1663=ADVANCED_FACE('',(#256,#155),#175,.T.);
#1664=ADVANCED_FACE('',(#257),#176,.T.);
#1665=ADVANCED_FACE('',(#258),#177,.F.);
#1666=ADVANCED_FACE('',(#259),#178,.F.);
#1667=ADVANCED_FACE('',(#260),#179,.F.);
#1668=ADVANCED_FACE('',(#261,#156),#180,.T.);
#1669=ADVANCED_FACE('',(#262),#1608,.F.);
#1670=ADVANCED_FACE('',(#263),#1609,.F.);
#1671=ADVANCED_FACE('',(#264),#181,.T.);
#1672=ADVANCED_FACE('',(#265,#157),#182,.T.);
#1673=ADVANCED_FACE('',(#266),#183,.T.);
#1674=ADVANCED_FACE('',(#267),#184,.T.);
#1675=ADVANCED_FACE('',(#268),#185,.F.);
#1676=ADVANCED_FACE('',(#269),#186,.F.);
#1677=ADVANCED_FACE('',(#270),#187,.F.);
#1678=ADVANCED_FACE('',(#271),#188,.F.);
#1679=ADVANCED_FACE('',(#272),#189,.F.);
#1680=ADVANCED_FACE('',(#273),#190,.F.);
#1681=ADVANCED_FACE('',(#274),#191,.F.);
#1682=ADVANCED_FACE('',(#275),#192,.F.);
#1683=ADVANCED_FACE('',(#276),#193,.F.);
#1684=ADVANCED_FACE('',(#277),#194,.F.);
#1685=ADVANCED_FACE('',(#278),#195,.T.);
#1686=ADVANCED_FACE('',(#279),#57,.T.);
#1687=ADVANCED_FACE('',(#280),#1610,.T.);
#1688=ADVANCED_FACE('',(#281),#58,.T.);
#1689=ADVANCED_FACE('',(#282,#158),#196,.T.);
#1690=ADVANCED_FACE('',(#283),#59,.T.);
#1691=ADVANCED_FACE('',(#284),#1611,.T.);
#1692=ADVANCED_FACE('',(#285),#1612,.F.);
#1693=ADVANCED_FACE('',(#286),#1613,.T.);
#1694=ADVANCED_FACE('',(#287,#159),#197,.T.);
#1695=ADVANCED_FACE('',(#288,#160),#198,.F.);
#1696=ADVANCED_FACE('',(#289),#1614,.T.);
#1697=ADVANCED_FACE('',(#290),#60,.T.);
#1698=ADVANCED_FACE('',(#291),#199,.T.);
#1699=ADVANCED_FACE('',(#292),#61,.T.);
#1700=ADVANCED_FACE('',(#293),#200,.T.);
#1701=ADVANCED_FACE('',(#294),#201,.T.);
#1702=ADVANCED_FACE('',(#295),#202,.T.);
#1703=ADVANCED_FACE('',(#296),#203,.T.);
#1704=ADVANCED_FACE('',(#297),#204,.T.);
#1705=ADVANCED_FACE('',(#298),#205,.T.);
#1706=ADVANCED_FACE('',(#299),#206,.T.);
#1707=ADVANCED_FACE('',(#300,#161),#207,.F.);
#1708=CLOSED_SHELL('',(#1615,#1616,#1617,#1618,#1619,#1620,#1621,#1622,
#1623,#1624,#1625,#1626,#1627,#1628,#1629,#1630,#1631,#1632,#1633,#1634,
#1635,#1636,#1637,#1638,#1639,#1640,#1641,#1642,#1643,#1644,#1645,#1646,
#1647,#1648,#1649,#1650));
#1709=CLOSED_SHELL('',(#1651,#1652,#1653,#1654,#1655,#1656,#1657,#1658,
#1659,#1660,#1661,#1662,#1663,#1664,#1665));
#1710=CLOSED_SHELL('',(#1666,#1667,#1668,#1669,#1670,#1671,#1672,#1673,
#1674,#1675));
#1711=CLOSED_SHELL('',(#1676,#1677,#1678,#1679,#1680,#1681,#1682,#1683));
#1712=CLOSED_SHELL('',(#1684,#1685,#1686,#1687,#1688,#1689,#1690,#1691));
#1713=CLOSED_SHELL('',(#1692,#1693,#1694,#1695));
#1714=CLOSED_SHELL('',(#1696,#1697,#1698,#1699,#1700,#1701,#1702,#1703,
#1704,#1705,#1706,#1707));
#1715=DERIVED_UNIT_ELEMENT(#1727,1.);
#1716=DERIVED_UNIT_ELEMENT(#2998,-3.);
#1717=DERIVED_UNIT_ELEMENT(#1727,1.);
#1718=DERIVED_UNIT_ELEMENT(#2998,-3.);
#1719=DERIVED_UNIT_ELEMENT(#1727,1.);
#1720=DERIVED_UNIT_ELEMENT(#2998,-3.);
#1721=DERIVED_UNIT_ELEMENT(#1727,1.);
#1722=DERIVED_UNIT_ELEMENT(#2998,-3.);
#1723=DERIVED_UNIT_ELEMENT(#1727,1.);
#1724=DERIVED_UNIT_ELEMENT(#2998,-3.);
#1725=DERIVED_UNIT_ELEMENT(#1727,1.);
#1726=DERIVED_UNIT_ELEMENT(#2998,-3.);
#1727=(
MASS_UNIT()
NAMED_UNIT(*)
SI_UNIT(.KILO.,.GRAM.)
);
#1728=DERIVED_UNIT((#1715,#1716));
#1729=DERIVED_UNIT((#1717,#1718));
#1730=DERIVED_UNIT((#1719,#1720));
#1731=DERIVED_UNIT((#1721,#1722));
#1732=DERIVED_UNIT((#1723,#1724));
#1733=DERIVED_UNIT((#1725,#1726));
#1734=MEASURE_REPRESENTATION_ITEM('density measure',
POSITIVE_RATIO_MEASURE(7850.),#1728);
#1735=MEASURE_REPRESENTATION_ITEM('density measure',
POSITIVE_RATIO_MEASURE(7850.),#1729);
#1736=MEASURE_REPRESENTATION_ITEM('density measure',
POSITIVE_RATIO_MEASURE(7850.),#1730);
#1737=MEASURE_REPRESENTATION_ITEM('density measure',
POSITIVE_RATIO_MEASURE(7850.),#1731);
#1738=MEASURE_REPRESENTATION_ITEM('density measure',
POSITIVE_RATIO_MEASURE(7850.),#1732);
#1739=MEASURE_REPRESENTATION_ITEM('density measure',
POSITIVE_RATIO_MEASURE(7850.),#1733);
#1740=PROPERTY_DEFINITION_REPRESENTATION(#1770,#1752);
#1741=PROPERTY_DEFINITION_REPRESENTATION(#1771,#1753);
#1742=PROPERTY_DEFINITION_REPRESENTATION(#1772,#1754);
#1743=PROPERTY_DEFINITION_REPRESENTATION(#1773,#1755);
#1744=PROPERTY_DEFINITION_REPRESENTATION(#1774,#1756);
#1745=PROPERTY_DEFINITION_REPRESENTATION(#1775,#1757);
#1746=PROPERTY_DEFINITION_REPRESENTATION(#1776,#1758);
#1747=PROPERTY_DEFINITION_REPRESENTATION(#1777,#1759);
#1748=PROPERTY_DEFINITION_REPRESENTATION(#1778,#1760);
#1749=PROPERTY_DEFINITION_REPRESENTATION(#1779,#1761);
#1750=PROPERTY_DEFINITION_REPRESENTATION(#1780,#1762);
#1751=PROPERTY_DEFINITION_REPRESENTATION(#1781,#1763);
#1752=REPRESENTATION('material name',(#1764),#2990);
#1753=REPRESENTATION('density',(#1734),#2990);
#1754=REPRESENTATION('material name',(#1765),#2991);
#1755=REPRESENTATION('density',(#1735),#2991);
#1756=REPRESENTATION('material name',(#1766),#2992);
#1757=REPRESENTATION('density',(#1736),#2992);
#1758=REPRESENTATION('material name',(#1767),#2993);
#1759=REPRESENTATION('density',(#1737),#2993);
#1760=REPRESENTATION('material name',(#1768),#2994);
#1761=REPRESENTATION('density',(#1738),#2994);
#1762=REPRESENTATION('material name',(#1769),#2995);
#1763=REPRESENTATION('density',(#1739),#2995);
#1764=DESCRIPTIVE_REPRESENTATION_ITEM('Steel','Steel');
#1765=DESCRIPTIVE_REPRESENTATION_ITEM('Steel','Steel');
#1766=DESCRIPTIVE_REPRESENTATION_ITEM('Steel','Steel');
#1767=DESCRIPTIVE_REPRESENTATION_ITEM('Steel','Steel');
#1768=DESCRIPTIVE_REPRESENTATION_ITEM('Steel','Steel');
#1769=DESCRIPTIVE_REPRESENTATION_ITEM('Steel','Steel');
#1770=PROPERTY_DEFINITION('material property','material name',#3038);
#1771=PROPERTY_DEFINITION('material property','density of part',#3038);
#1772=PROPERTY_DEFINITION('material property','material name',#3039);
#1773=PROPERTY_DEFINITION('material property','density of part',#3039);
#1774=PROPERTY_DEFINITION('material property','material name',#3040);
#1775=PROPERTY_DEFINITION('material property','density of part',#3040);
#1776=PROPERTY_DEFINITION('material property','material name',#3041);
#1777=PROPERTY_DEFINITION('material property','density of part',#3041);
#1778=PROPERTY_DEFINITION('material property','material name',#3042);
#1779=PROPERTY_DEFINITION('material property','density of part',#3042);
#1780=PROPERTY_DEFINITION('material property','material name',#3043);
#1781=PROPERTY_DEFINITION('material property','density of part',#3043);
#1782=AXIS2_PLACEMENT_3D('',#2501,#1982,#1983);
#1783=AXIS2_PLACEMENT_3D('',#2502,#1984,#1985);
#1784=AXIS2_PLACEMENT_3D('',#2503,#1986,#1987);
#1785=AXIS2_PLACEMENT_3D('',#2504,#1988,#1989);
#1786=AXIS2_PLACEMENT_3D('',#2506,#1990,#1991);
#1787=AXIS2_PLACEMENT_3D('',#2509,#1993,#1994);
#1788=AXIS2_PLACEMENT_3D('',#2510,#1995,#1996);
#1789=AXIS2_PLACEMENT_3D('',#2512,#1997,#1998);
#1790=AXIS2_PLACEMENT_3D('',#2515,#2000,#2001);
#1791=AXIS2_PLACEMENT_3D('',#2516,#2002,#2003);
#1792=AXIS2_PLACEMENT_3D('',#2518,#2004,#2005);
#1793=AXIS2_PLACEMENT_3D('',#2521,#2007,#2008);
#1794=AXIS2_PLACEMENT_3D('',#2522,#2009,#2010);
#1795=AXIS2_PLACEMENT_3D('',#2524,#2011,#2012);
#1796=AXIS2_PLACEMENT_3D('',#2527,#2014,#2015);
#1797=AXIS2_PLACEMENT_3D('',#2528,#2016,#2017);
#1798=AXIS2_PLACEMENT_3D('',#2530,#2018,#2019);
#1799=AXIS2_PLACEMENT_3D('',#2533,#2021,#2022);
#1800=AXIS2_PLACEMENT_3D('',#2534,#2023,#2024);
#1801=AXIS2_PLACEMENT_3D('',#2536,#2025,#2026);
#1802=AXIS2_PLACEMENT_3D('',#2539,#2028,#2029);
#1803=AXIS2_PLACEMENT_3D('',#2540,#2030,#2031);
#1804=AXIS2_PLACEMENT_3D('',#2542,#2032,#2033);
#1805=AXIS2_PLACEMENT_3D('',#2545,#2035,#2036);
#1806=AXIS2_PLACEMENT_3D('',#2546,#2037,#2038);
#1807=AXIS2_PLACEMENT_3D('',#2548,#2039,#2040);
#1808=AXIS2_PLACEMENT_3D('',#2551,#2042,#2043);
#1809=AXIS2_PLACEMENT_3D('',#2552,#2044,#2045);
#1810=AXIS2_PLACEMENT_3D('',#2554,#2046,#2047);
#1811=AXIS2_PLACEMENT_3D('',#2557,#2049,#2050);
#1812=AXIS2_PLACEMENT_3D('',#2558,#2051,#2052);
#1813=AXIS2_PLACEMENT_3D('',#2560,#2053,#2054);
#1814=AXIS2_PLACEMENT_3D('',#2563,#2056,#2057);
#1815=AXIS2_PLACEMENT_3D('',#2564,#2058,#2059);
#1816=AXIS2_PLACEMENT_3D('',#2566,#2060,#2061);
#1817=AXIS2_PLACEMENT_3D('',#2569,#2063,#2064);
#1818=AXIS2_PLACEMENT_3D('',#2570,#2065,#2066);
#1819=AXIS2_PLACEMENT_3D('',#2572,#2067,#2068);
#1820=AXIS2_PLACEMENT_3D('',#2575,#2070,#2071);
#1821=AXIS2_PLACEMENT_3D('',#2576,#2072,#2073);
#1822=AXIS2_PLACEMENT_3D('',#2578,#2074,#2075);
#1823=AXIS2_PLACEMENT_3D('',#2581,#2077,#2078);
#1824=AXIS2_PLACEMENT_3D('',#2582,#2079,#2080);
#1825=AXIS2_PLACEMENT_3D('',#2584,#2081,#2082);
#1826=AXIS2_PLACEMENT_3D('',#2587,#2084,#2085);
#1827=AXIS2_PLACEMENT_3D('',#2588,#2086,#2087);
#1828=AXIS2_PLACEMENT_3D('',#2590,#2088,#2089);
#1829=AXIS2_PLACEMENT_3D('',#2593,#2091,#2092);
#1830=AXIS2_PLACEMENT_3D('',#2594,#2093,#2094);
#1831=AXIS2_PLACEMENT_3D('',#2596,#2095,#2096);
#1832=AXIS2_PLACEMENT_3D('',#2599,#2098,#2099);
#1833=AXIS2_PLACEMENT_3D('',#2600,#2100,#2101);
#1834=AXIS2_PLACEMENT_3D('',#2602,#2102,#2103);
#1835=AXIS2_PLACEMENT_3D('',#2605,#2105,#2106);
#1836=AXIS2_PLACEMENT_3D('',#2606,#2107,#2108);
#1837=AXIS2_PLACEMENT_3D('',#2608,#2109,#2110);
#1838=AXIS2_PLACEMENT_3D('',#2611,#2112,#2113);
#1839=AXIS2_PLACEMENT_3D('',#2612,#2114,#2115);
#1840=AXIS2_PLACEMENT_3D('',#2614,#2116,#2117);
#1841=AXIS2_PLACEMENT_3D('',#2617,#2119,#2120);
#1842=AXIS2_PLACEMENT_3D('',#2618,#2121,#2122);
#1843=AXIS2_PLACEMENT_3D('',#2620,#2123,#2124);
#1844=AXIS2_PLACEMENT_3D('',#2623,#2126,#2127);
#1845=AXIS2_PLACEMENT_3D('',#2624,#2128,#2129);
#1846=AXIS2_PLACEMENT_3D('',#2626,#2130,#2131);
#1847=AXIS2_PLACEMENT_3D('',#2629,#2133,#2134);
#1848=AXIS2_PLACEMENT_3D('',#2630,#2135,#2136);
#1849=AXIS2_PLACEMENT_3D('',#2632,#2137,#2138);
#1850=AXIS2_PLACEMENT_3D('',#2635,#2140,#2141);
#1851=AXIS2_PLACEMENT_3D('',#2636,#2142,#2143);
#1852=AXIS2_PLACEMENT_3D('',#2638,#2144,#2145);
#1853=AXIS2_PLACEMENT_3D('',#2641,#2147,#2148);
#1854=AXIS2_PLACEMENT_3D('',#2642,#2149,#2150);
#1855=AXIS2_PLACEMENT_3D('',#2644,#2151,#2152);
#1856=AXIS2_PLACEMENT_3D('',#2647,#2154,#2155);
#1857=AXIS2_PLACEMENT_3D('',#2648,#2156,#2157);
#1858=AXIS2_PLACEMENT_3D('',#2650,#2158,#2159);
#1859=AXIS2_PLACEMENT_3D('',#2653,#2161,#2162);
#1860=AXIS2_PLACEMENT_3D('',#2654,#2163,#2164);
#1861=AXIS2_PLACEMENT_3D('',#2656,#2165,#2166);
#1862=AXIS2_PLACEMENT_3D('',#2659,#2168,#2169);
#1863=AXIS2_PLACEMENT_3D('',#2660,#2170,#2171);
#1864=AXIS2_PLACEMENT_3D('',#2662,#2172,#2173);
#1865=AXIS2_PLACEMENT_3D('',#2665,#2175,#2176);
#1866=AXIS2_PLACEMENT_3D('',#2666,#2177,#2178);
#1867=AXIS2_PLACEMENT_3D('',#2668,#2179,#2180);
#1868=AXIS2_PLACEMENT_3D('',#2671,#2182,#2183);
#1869=AXIS2_PLACEMENT_3D('',#2672,#2184,#2185);
#1870=AXIS2_PLACEMENT_3D('',#2674,#2186,#2187);
#1871=AXIS2_PLACEMENT_3D('',#2677,#2189,#2190);
#1872=AXIS2_PLACEMENT_3D('',#2678,#2191,#2192);
#1873=AXIS2_PLACEMENT_3D('',#2680,#2193,#2194);
#1874=AXIS2_PLACEMENT_3D('',#2683,#2196,#2197);
#1875=AXIS2_PLACEMENT_3D('',#2684,#2198,#2199);
#1876=AXIS2_PLACEMENT_3D('',#2693,#2204,#2205);
#1877=AXIS2_PLACEMENT_3D('',#2699,#2209,#2210);
#1878=AXIS2_PLACEMENT_3D('',#2705,#2214,#2215);
#1879=AXIS2_PLACEMENT_3D('',#2708,#2218,#2219);
#1880=AXIS2_PLACEMENT_3D('',#2709,#2220,#2221);
#1881=AXIS2_PLACEMENT_3D('',#2710,#2222,#2223);
#1882=AXIS2_PLACEMENT_3D('',#2711,#2224,#2225);
#1883=AXIS2_PLACEMENT_3D('',#2713,#2226,#2227);
#1884=AXIS2_PLACEMENT_3D('',#2716,#2229,#2230);
#1885=AXIS2_PLACEMENT_3D('',#2717,#2231,#2232);
#1886=AXIS2_PLACEMENT_3D('',#2718,#2233,#2234);
#1887=AXIS2_PLACEMENT_3D('',#2720,#2235,#2236);
#1888=AXIS2_PLACEMENT_3D('',#2723,#2238,#2239);
#1889=AXIS2_PLACEMENT_3D('',#2724,#2240,#2241);
#1890=AXIS2_PLACEMENT_3D('',#2725,#2242,#2243);
#1891=AXIS2_PLACEMENT_3D('',#2727,#2244,#2245);
#1892=AXIS2_PLACEMENT_3D('',#2730,#2247,#2248);
#1893=AXIS2_PLACEMENT_3D('',#2731,#2249,#2250);
#1894=AXIS2_PLACEMENT_3D('',#2732,#2251,#2252);
#1895=AXIS2_PLACEMENT_3D('',#2734,#2253,#2254);
#1896=AXIS2_PLACEMENT_3D('',#2737,#2256,#2257);
#1897=AXIS2_PLACEMENT_3D('',#2738,#2258,#2259);
#1898=AXIS2_PLACEMENT_3D('',#2739,#2260,#2261);
#1899=AXIS2_PLACEMENT_3D('',#2741,#2262,#2263);
#1900=AXIS2_PLACEMENT_3D('',#2744,#2265,#2266);
#1901=AXIS2_PLACEMENT_3D('',#2745,#2267,#2268);
#1902=AXIS2_PLACEMENT_3D('',#2754,#2273,#2274);
#1903=AXIS2_PLACEMENT_3D('',#2760,#2278,#2279);
#1904=AXIS2_PLACEMENT_3D('',#2766,#2283,#2284);
#1905=AXIS2_PLACEMENT_3D('',#2769,#2287,#2288);
#1906=AXIS2_PLACEMENT_3D('',#2770,#2289,#2290);
#1907=AXIS2_PLACEMENT_3D('',#2771,#2291,#2292);
#1908=AXIS2_PLACEMENT_3D('',#2772,#2293,#2294);
#1909=AXIS2_PLACEMENT_3D('',#2781,#2299,#2300);
#1910=AXIS2_PLACEMENT_3D('',#2790,#2305,#2306);
#1911=AXIS2_PLACEMENT_3D('',#2799,#2311,#2312);
#1912=AXIS2_PLACEMENT_3D('',#2800,#2313,#2314);
#1913=AXIS2_PLACEMENT_3D('',#2801,#2315,#2316);
#1914=AXIS2_PLACEMENT_3D('',#2802,#2317,#2318);
#1915=AXIS2_PLACEMENT_3D('',#2803,#2319,#2320);
#1916=AXIS2_PLACEMENT_3D('',#2804,#2321,#2322);
#1917=AXIS2_PLACEMENT_3D('',#2805,#2323,#2324);
#1918=AXIS2_PLACEMENT_3D('',#2811,#2328,#2329);
#1919=AXIS2_PLACEMENT_3D('',#2817,#2333,#2334);
#1920=AXIS2_PLACEMENT_3D('',#2820,#2337,#2338);
#1921=AXIS2_PLACEMENT_3D('',#2821,#2339,#2340);
#1922=AXIS2_PLACEMENT_3D('',#2822,#2341,#2342);
#1923=AXIS2_PLACEMENT_3D('',#2823,#2343,#2344);
#1924=AXIS2_PLACEMENT_3D('',#2832,#2349,#2350);
#1925=AXIS2_PLACEMENT_3D('',#2838,#2354,#2355);
#1926=AXIS2_PLACEMENT_3D('',#2844,#2359,#2360);
#1927=AXIS2_PLACEMENT_3D('',#2850,#2364,#2365);
#1928=AXIS2_PLACEMENT_3D('',#2856,#2369,#2370);
#1929=AXIS2_PLACEMENT_3D('',#2859,#2373,#2374);
#1930=AXIS2_PLACEMENT_3D('',#2860,#2375,#2376);
#1931=AXIS2_PLACEMENT_3D('',#2861,#2377,#2378);
#1932=AXIS2_PLACEMENT_3D('',#2863,#2379,#2380);
#1933=AXIS2_PLACEMENT_3D('',#2864,#2381,#2382);
#1934=AXIS2_PLACEMENT_3D('',#2866,#2383,#2384);
#1935=AXIS2_PLACEMENT_3D('',#2867,#2385,#2386);
#1936=AXIS2_PLACEMENT_3D('',#2869,#2387,#2388);
#1937=AXIS2_PLACEMENT_3D('',#2871,#2390,#2391);
#1938=AXIS2_PLACEMENT_3D('',#2873,#2392,#2393);
#1939=AXIS2_PLACEMENT_3D('',#2875,#2395,#2396);
#1940=AXIS2_PLACEMENT_3D('',#2877,#2397,#2398);
#1941=AXIS2_PLACEMENT_3D('',#2879,#2400,#2401);
#1942=AXIS2_PLACEMENT_3D('',#2881,#2402,#2403);
#1943=AXIS2_PLACEMENT_3D('',#2882,#2404,#2405);
#1944=AXIS2_PLACEMENT_3D('',#2884,#2406,#2407);
#1945=AXIS2_PLACEMENT_3D('',#2886,#2409,#2410);
#1946=AXIS2_PLACEMENT_3D('',#2888,#2412,#2413);
#1947=AXIS2_PLACEMENT_3D('',#2889,#2414,#2415);
#1948=AXIS2_PLACEMENT_3D('',#2891,#2416,#2417);
#1949=AXIS2_PLACEMENT_3D('',#2894,#2419,#2420);
#1950=AXIS2_PLACEMENT_3D('',#2895,#2421,#2422);
#1951=AXIS2_PLACEMENT_3D('',#2897,#2423,#2424);
#1952=AXIS2_PLACEMENT_3D('',#2900,#2426,#2427);
#1953=AXIS2_PLACEMENT_3D('',#2901,#2428,#2429);
#1954=AXIS2_PLACEMENT_3D('',#2902,#2430,#2431);
#1955=AXIS2_PLACEMENT_3D('',#2903,#2432,#2433);
#1956=AXIS2_PLACEMENT_3D('',#2904,#2434,#2435);
#1957=AXIS2_PLACEMENT_3D('',#2906,#2436,#2437);
#1958=AXIS2_PLACEMENT_3D('',#2909,#2439,#2440);
#1959=AXIS2_PLACEMENT_3D('',#2910,#2441,#2442);
#1960=AXIS2_PLACEMENT_3D('',#2912,#2443,#2444);
#1961=AXIS2_PLACEMENT_3D('',#2914,#2446,#2447);
#1962=AXIS2_PLACEMENT_3D('',#2915,#2448,#2449);
#1963=AXIS2_PLACEMENT_3D('',#2917,#2450,#2451);
#1964=AXIS2_PLACEMENT_3D('',#2943,#2453,#2454);
#1965=AXIS2_PLACEMENT_3D('',#2949,#2458,#2459);
#1966=AXIS2_PLACEMENT_3D('',#2953,#2462,#2463);
#1967=AXIS2_PLACEMENT_3D('',#2957,#2466,#2467);
#1968=AXIS2_PLACEMENT_3D('',#2961,#2470,#2471);
#1969=AXIS2_PLACEMENT_3D('',#2965,#2474,#2475);
#1970=AXIS2_PLACEMENT_3D('',#2967,#2477,#2478);
#1971=AXIS2_PLACEMENT_3D('',#2968,#2479,#2480);
#1972=AXIS2_PLACEMENT_3D('',#2969,#2481,#2482);
#1973=AXIS2_PLACEMENT_3D('',#2970,#2483,#2484);
#1974=AXIS2_PLACEMENT_3D('',#2971,#2485,#2486);
#1975=AXIS2_PLACEMENT_3D('',#2972,#2487,#2488);
#1976=AXIS2_PLACEMENT_3D('',#2973,#2489,#2490);
#1977=AXIS2_PLACEMENT_3D('',#2974,#2491,#2492);
#1978=AXIS2_PLACEMENT_3D('',#2975,#2493,#2494);
#1979=AXIS2_PLACEMENT_3D('',#2976,#2495,#2496);
#1980=AXIS2_PLACEMENT_3D('',#2977,#2497,#2498);
#1981=AXIS2_PLACEMENT_3D('',#2978,#2499,#2500);
#1982=DIRECTION('axis',(0.,0.,1.));
#1983=DIRECTION('refdir',(1.,0.,0.));
#1984=DIRECTION('axis',(0.,0.,1.));
#1985=DIRECTION('refdir',(1.,0.,0.));
#1986=DIRECTION('axis',(0.,0.,1.));
#1987=DIRECTION('refdir',(1.,0.,0.));
#1988=DIRECTION('center_axis',(0.,0.,1.));
#1989=DIRECTION('ref_axis',(1.,0.,0.));
#1990=DIRECTION('center_axis',(0.,0.,1.));
#1991=DIRECTION('ref_axis',(1.,0.,0.));
#1992=DIRECTION('',(0.,0.,1.));
#1993=DIRECTION('center_axis',(0.,0.,-1.));
#1994=DIRECTION('ref_axis',(1.,0.,0.));
#1995=DIRECTION('center_axis',(0.,0.,1.));
#1996=DIRECTION('ref_axis',(1.,0.,0.));
#1997=DIRECTION('center_axis',(0.,0.,1.));
#1998=DIRECTION('ref_axis',(1.,0.,0.));
#1999=DIRECTION('',(0.,0.,1.));
#2000=DIRECTION('center_axis',(0.,0.,-1.));
#2001=DIRECTION('ref_axis',(1.,0.,0.));
#2002=DIRECTION('center_axis',(0.,0.,1.));
#2003=DIRECTION('ref_axis',(1.,0.,0.));
#2004=DIRECTION('center_axis',(0.,0.,1.));
#2005=DIRECTION('ref_axis',(1.,0.,0.));
#2006=DIRECTION('',(0.,0.,1.));
#2007=DIRECTION('center_axis',(0.,0.,-1.));
#2008=DIRECTION('ref_axis',(1.,0.,0.));
#2009=DIRECTION('center_axis',(0.,0.,1.));
#2010=DIRECTION('ref_axis',(1.,0.,0.));
#2011=DIRECTION('center_axis',(0.,0.,1.));
#2012=DIRECTION('ref_axis',(1.,0.,0.));
#2013=DIRECTION('',(0.,0.,1.));
#2014=DIRECTION('center_axis',(0.,0.,-1.));
#2015=DIRECTION('ref_axis',(1.,0.,0.));
#2016=DIRECTION('center_axis',(0.,0.,1.));
#2017=DIRECTION('ref_axis',(1.,0.,0.));
#2018=DIRECTION('center_axis',(0.,0.,1.));
#2019=DIRECTION('ref_axis',(1.,0.,0.));
#2020=DIRECTION('',(0.,0.,1.));
#2021=DIRECTION('center_axis',(0.,0.,-1.));
#2022=DIRECTION('ref_axis',(1.,0.,0.));
#2023=DIRECTION('center_axis',(0.,0.,1.));
#2024=DIRECTION('ref_axis',(1.,0.,0.));
#2025=DIRECTION('center_axis',(0.,0.,1.));
#2026=DIRECTION('ref_axis',(1.,0.,0.));
#2027=DIRECTION('',(0.,0.,1.));
#2028=DIRECTION('center_axis',(0.,0.,-1.));
#2029=DIRECTION('ref_axis',(1.,0.,0.));
#2030=DIRECTION('center_axis',(0.,0.,1.));
#2031=DIRECTION('ref_axis',(1.,0.,0.));
#2032=DIRECTION('center_axis',(0.,0.,1.));
#2033=DIRECTION('ref_axis',(1.,0.,0.));
#2034=DIRECTION('',(0.,0.,1.));
#2035=DIRECTION('center_axis',(0.,0.,-1.));
#2036=DIRECTION('ref_axis',(1.,0.,0.));
#2037=DIRECTION('center_axis',(0.,0.,1.));
#2038=DIRECTION('ref_axis',(1.,0.,0.));
#2039=DIRECTION('center_axis',(0.,0.,1.));
#2040=DIRECTION('ref_axis',(1.,0.,0.));
#2041=DIRECTION('',(0.,0.,1.));
#2042=DIRECTION('center_axis',(0.,0.,-1.));
#2043=DIRECTION('ref_axis',(1.,0.,0.));
#2044=DIRECTION('center_axis',(0.,0.,1.));
#2045=DIRECTION('ref_axis',(1.,0.,0.));
#2046=DIRECTION('center_axis',(0.,0.,1.));
#2047=DIRECTION('ref_axis',(1.,0.,0.));
#2048=DIRECTION('',(0.,0.,1.));
#2049=DIRECTION('center_axis',(0.,0.,-1.));
#2050=DIRECTION('ref_axis',(1.,0.,0.));
#2051=DIRECTION('center_axis',(0.,0.,1.));
#2052=DIRECTION('ref_axis',(1.,0.,0.));
#2053=DIRECTION('center_axis',(0.,0.,1.));
#2054=DIRECTION('ref_axis',(1.,0.,0.));
#2055=DIRECTION('',(0.,0.,1.));
#2056=DIRECTION('center_axis',(0.,0.,-1.));
#2057=DIRECTION('ref_axis',(1.,0.,0.));
#2058=DIRECTION('center_axis',(0.,0.,1.));
#2059=DIRECTION('ref_axis',(1.,0.,0.));
#2060=DIRECTION('center_axis',(0.,0.,1.));
#2061=DIRECTION('ref_axis',(1.,0.,0.));
#2062=DIRECTION('',(0.,0.,1.));
#2063=DIRECTION('center_axis',(0.,0.,-1.));
#2064=DIRECTION('ref_axis',(1.,0.,0.));
#2065=DIRECTION('center_axis',(0.,0.,1.));
#2066=DIRECTION('ref_axis',(1.,0.,0.));
#2067=DIRECTION('center_axis',(0.,0.,1.));
#2068=DIRECTION('ref_axis',(1.,0.,0.));
#2069=DIRECTION('',(0.,0.,1.));
#2070=DIRECTION('center_axis',(0.,0.,-1.));
#2071=DIRECTION('ref_axis',(1.,0.,0.));
#2072=DIRECTION('center_axis',(0.,0.,1.));
#2073=DIRECTION('ref_axis',(1.,0.,0.));
#2074=DIRECTION('center_axis',(0.,0.,1.));
#2075=DIRECTION('ref_axis',(1.,0.,0.));
#2076=DIRECTION('',(0.,0.,1.));
#2077=DIRECTION('center_axis',(0.,0.,-1.));
#2078=DIRECTION('ref_axis',(1.,0.,0.));
#2079=DIRECTION('center_axis',(0.,0.,1.));
#2080=DIRECTION('ref_axis',(1.,0.,0.));
#2081=DIRECTION('center_axis',(0.,0.,1.));
#2082=DIRECTION('ref_axis',(1.,0.,0.));
#2083=DIRECTION('',(0.,0.,1.));
#2084=DIRECTION('center_axis',(0.,0.,-1.));
#2085=DIRECTION('ref_axis',(1.,0.,0.));
#2086=DIRECTION('center_axis',(0.,0.,1.));
#2087=DIRECTION('ref_axis',(1.,0.,0.));
#2088=DIRECTION('center_axis',(0.,0.,1.));
#2089=DIRECTION('ref_axis',(1.,0.,0.));
#2090=DIRECTION('',(0.,0.,1.));
#2091=DIRECTION('center_axis',(0.,0.,-1.));
#2092=DIRECTION('ref_axis',(1.,0.,0.));
#2093=DIRECTION('center_axis',(0.,0.,1.));
#2094=DIRECTION('ref_axis',(1.,0.,0.));
#2095=DIRECTION('center_axis',(0.,0.,1.));
#2096=DIRECTION('ref_axis',(1.,0.,0.));
#2097=DIRECTION('',(0.,0.,1.));
#2098=DIRECTION('center_axis',(0.,0.,-1.));
#2099=DIRECTION('ref_axis',(1.,0.,0.));
#2100=DIRECTION('center_axis',(0.,0.,1.));
#2101=DIRECTION('ref_axis',(1.,0.,0.));
#2102=DIRECTION('center_axis',(0.,0.,1.));
#2103=DIRECTION('ref_axis',(1.,0.,0.));
#2104=DIRECTION('',(0.,0.,1.));
#2105=DIRECTION('center_axis',(0.,0.,-1.));
#2106=DIRECTION('ref_axis',(1.,0.,0.));
#2107=DIRECTION('center_axis',(0.,0.,1.));
#2108=DIRECTION('ref_axis',(1.,0.,0.));
#2109=DIRECTION('center_axis',(0.,0.,1.));
#2110=DIRECTION('ref_axis',(1.,0.,0.));
#2111=DIRECTION('',(0.,0.,1.));
#2112=DIRECTION('center_axis',(0.,0.,-1.));
#2113=DIRECTION('ref_axis',(1.,0.,0.));
#2114=DIRECTION('center_axis',(0.,0.,1.));
#2115=DIRECTION('ref_axis',(1.,0.,0.));
#2116=DIRECTION('center_axis',(0.,0.,1.));
#2117=DIRECTION('ref_axis',(1.,0.,0.));
#2118=DIRECTION('',(0.,0.,1.));
#2119=DIRECTION('center_axis',(0.,0.,-1.));
#2120=DIRECTION('ref_axis',(1.,0.,0.));
#2121=DIRECTION('center_axis',(0.,0.,1.));
#2122=DIRECTION('ref_axis',(1.,0.,0.));
#2123=DIRECTION('center_axis',(0.,0.,1.));
#2124=DIRECTION('ref_axis',(1.,0.,0.));
#2125=DIRECTION('',(0.,0.,1.));
#2126=DIRECTION('center_axis',(0.,0.,-1.));
#2127=DIRECTION('ref_axis',(1.,0.,0.));
#2128=DIRECTION('center_axis',(0.,0.,1.));
#2129=DIRECTION('ref_axis',(1.,0.,0.));
#2130=DIRECTION('center_axis',(0.,0.,1.));
#2131=DIRECTION('ref_axis',(1.,0.,0.));
#2132=DIRECTION('',(0.,0.,1.));
#2133=DIRECTION('center_axis',(0.,0.,-1.));
#2134=DIRECTION('ref_axis',(1.,0.,0.));
#2135=DIRECTION('center_axis',(0.,0.,1.));
#2136=DIRECTION('ref_axis',(1.,0.,0.));
#2137=DIRECTION('center_axis',(0.,0.,1.));
#2138=DIRECTION('ref_axis',(1.,0.,0.));
#2139=DIRECTION('',(0.,0.,1.));
#2140=DIRECTION('center_axis',(0.,0.,-1.));
#2141=DIRECTION('ref_axis',(1.,0.,0.));
#2142=DIRECTION('center_axis',(0.,0.,1.));
#2143=DIRECTION('ref_axis',(1.,0.,0.));
#2144=DIRECTION('center_axis',(0.,0.,1.));
#2145=DIRECTION('ref_axis',(1.,0.,0.));
#2146=DIRECTION('',(0.,0.,1.));
#2147=DIRECTION('center_axis',(0.,0.,-1.));
#2148=DIRECTION('ref_axis',(1.,0.,0.));
#2149=DIRECTION('center_axis',(0.,0.,1.));
#2150=DIRECTION('ref_axis',(1.,0.,0.));
#2151=DIRECTION('center_axis',(0.,0.,1.));
#2152=DIRECTION('ref_axis',(1.,0.,0.));
#2153=DIRECTION('',(0.,0.,1.));
#2154=DIRECTION('center_axis',(0.,0.,-1.));
#2155=DIRECTION('ref_axis',(1.,0.,0.));
#2156=DIRECTION('center_axis',(0.,0.,1.));
#2157=DIRECTION('ref_axis',(1.,0.,0.));
#2158=DIRECTION('center_axis',(0.,0.,1.));
#2159=DIRECTION('ref_axis',(1.,0.,0.));
#2160=DIRECTION('',(0.,0.,1.));
#2161=DIRECTION('center_axis',(0.,0.,-1.));
#2162=DIRECTION('ref_axis',(1.,0.,0.));
#2163=DIRECTION('center_axis',(0.,0.,1.));
#2164=DIRECTION('ref_axis',(1.,0.,0.));
#2165=DIRECTION('center_axis',(0.,0.,1.));
#2166=DIRECTION('ref_axis',(1.,0.,0.));
#2167=DIRECTION('',(0.,0.,1.));
#2168=DIRECTION('center_axis',(0.,0.,-1.));
#2169=DIRECTION('ref_axis',(1.,0.,0.));
#2170=DIRECTION('center_axis',(0.,0.,1.));
#2171=DIRECTION('ref_axis',(1.,0.,0.));
#2172=DIRECTION('center_axis',(0.,0.,1.));
#2173=DIRECTION('ref_axis',(1.,0.,0.));
#2174=DIRECTION('',(0.,0.,1.));
#2175=DIRECTION('center_axis',(0.,0.,-1.));
#2176=DIRECTION('ref_axis',(1.,0.,0.));
#2177=DIRECTION('center_axis',(0.,0.,1.));
#2178=DIRECTION('ref_axis',(1.,0.,0.));
#2179=DIRECTION('center_axis',(0.,0.,1.));
#2180=DIRECTION('ref_axis',(1.,0.,0.));
#2181=DIRECTION('',(0.,0.,1.));
#2182=DIRECTION('center_axis',(0.,0.,-1.));
#2183=DIRECTION('ref_axis',(1.,0.,0.));
#2184=DIRECTION('center_axis',(0.,0.,1.));
#2185=DIRECTION('ref_axis',(1.,0.,0.));
#2186=DIRECTION('center_axis',(0.,0.,1.));
#2187=DIRECTION('ref_axis',(1.,0.,0.));
#2188=DIRECTION('',(0.,0.,1.));
#2189=DIRECTION('center_axis',(0.,0.,-1.));
#2190=DIRECTION('ref_axis',(1.,0.,0.));
#2191=DIRECTION('center_axis',(0.,0.,1.));
#2192=DIRECTION('ref_axis',(1.,0.,0.));
#2193=DIRECTION('center_axis',(0.,0.,1.));
#2194=DIRECTION('ref_axis',(1.,0.,0.));
#2195=DIRECTION('',(0.,0.,1.));
#2196=DIRECTION('center_axis',(0.,0.,-1.));
#2197=DIRECTION('ref_axis',(1.,0.,0.));
#2198=DIRECTION('center_axis',(0.,1.,0.));
#2199=DIRECTION('ref_axis',(-1.,0.,0.));
#2200=DIRECTION('',(-1.,0.,0.));
#2201=DIRECTION('',(0.,0.,1.));
#2202=DIRECTION('',(-1.,0.,0.));
#2203=DIRECTION('',(0.,0.,1.));
#2204=DIRECTION('center_axis',(1.,0.,0.));
#2205=DIRECTION('ref_axis',(0.,1.,0.));
#2206=DIRECTION('',(0.,1.,0.));
#2207=DIRECTION('',(0.,1.,0.));
#2208=DIRECTION('',(0.,0.,1.));
#2209=DIRECTION('center_axis',(0.,-1.,0.));
#2210=DIRECTION('ref_axis',(1.,0.,0.));
#2211=DIRECTION('',(1.,0.,0.));
#2212=DIRECTION('',(1.,0.,0.));
#2213=DIRECTION('',(0.,0.,1.));
#2214=DIRECTION('center_axis',(-1.,0.,0.));
#2215=DIRECTION('ref_axis',(0.,-1.,0.));
#2216=DIRECTION('',(0.,-1.,0.));
#2217=DIRECTION('',(0.,-1.,0.));
#2218=DIRECTION('center_axis',(0.,0.,1.));
#2219=DIRECTION('ref_axis',(1.,0.,0.));
#2220=DIRECTION('center_axis',(0.,0.,1.));
#2221=DIRECTION('ref_axis',(1.,0.,0.));
#2222=DIRECTION('axis',(0.,0.,1.));
#2223=DIRECTION('refdir',(1.,0.,0.));
#2224=DIRECTION('center_axis',(0.,0.,1.));
#2225=DIRECTION('ref_axis',(1.,0.,0.));
#2226=DIRECTION('center_axis',(0.,0.,1.));
#2227=DIRECTION('ref_axis',(1.,0.,0.));
#2228=DIRECTION('',(0.,0.,1.));
#2229=DIRECTION('center_axis',(0.,0.,1.));
#2230=DIRECTION('ref_axis',(1.,0.,0.));
#2231=DIRECTION('center_axis',(0.,0.,1.));
#2232=DIRECTION('ref_axis',(1.,0.,0.));
#2233=DIRECTION('center_axis',(0.,0.,1.));
#2234=DIRECTION('ref_axis',(1.,0.,0.));
#2235=DIRECTION('center_axis',(0.,0.,1.));
#2236=DIRECTION('ref_axis',(1.,0.,0.));
#2237=DIRECTION('',(0.,0.,1.));
#2238=DIRECTION('center_axis',(0.,0.,1.));
#2239=DIRECTION('ref_axis',(1.,0.,0.));
#2240=DIRECTION('center_axis',(0.,0.,1.));
#2241=DIRECTION('ref_axis',(1.,0.,0.));
#2242=DIRECTION('center_axis',(0.,0.,1.));
#2243=DIRECTION('ref_axis',(1.,0.,0.));
#2244=DIRECTION('center_axis',(0.,0.,1.));
#2245=DIRECTION('ref_axis',(1.,0.,0.));
#2246=DIRECTION('',(0.,0.,1.));
#2247=DIRECTION('center_axis',(0.,0.,1.));
#2248=DIRECTION('ref_axis',(1.,0.,0.));
#2249=DIRECTION('center_axis',(0.,0.,1.));
#2250=DIRECTION('ref_axis',(1.,0.,0.));
#2251=DIRECTION('center_axis',(0.,0.,1.));
#2252=DIRECTION('ref_axis',(1.,0.,0.));
#2253=DIRECTION('center_axis',(0.,0.,1.));
#2254=DIRECTION('ref_axis',(1.,0.,0.));
#2255=DIRECTION('',(0.,0.,1.));
#2256=DIRECTION('center_axis',(0.,0.,1.));
#2257=DIRECTION('ref_axis',(1.,0.,0.));
#2258=DIRECTION('center_axis',(0.,0.,1.));
#2259=DIRECTION('ref_axis',(1.,0.,0.));
#2260=DIRECTION('center_axis',(0.,0.,1.));
#2261=DIRECTION('ref_axis',(1.,0.,0.));
#2262=DIRECTION('center_axis',(0.,0.,1.));
#2263=DIRECTION('ref_axis',(1.,0.,0.));
#2264=DIRECTION('',(0.,0.,1.));
#2265=DIRECTION('center_axis',(0.447213595499958,0.,-0.894427190999916));
#2266=DIRECTION('ref_axis',(0.894427190999916,0.,0.447213595499958));
#2267=DIRECTION('center_axis',(-1.,0.,0.));
#2268=DIRECTION('ref_axis',(0.,0.,1.));
#2269=DIRECTION('',(0.,0.,-1.));
#2270=DIRECTION('',(0.,1.,0.));
#2271=DIRECTION('',(0.,0.,1.));
#2272=DIRECTION('',(0.,1.,0.));
#2273=DIRECTION('center_axis',(0.,0.,-1.));
#2274=DIRECTION('ref_axis',(-1.,0.,0.));
#2275=DIRECTION('',(1.,0.,0.));
#2276=DIRECTION('',(-1.,0.,0.));
#2277=DIRECTION('',(0.,1.,0.));
#2278=DIRECTION('center_axis',(1.,0.,0.));
#2279=DIRECTION('ref_axis',(0.,0.,-1.));
#2280=DIRECTION('',(0.,0.,1.));
#2281=DIRECTION('',(0.,0.,-1.));
#2282=DIRECTION('',(0.,1.,0.));
#2283=DIRECTION('center_axis',(-0.447213595499958,0.,0.894427190999916));
#2284=DIRECTION('ref_axis',(0.894427190999916,0.,0.447213595499958));
#2285=DIRECTION('',(-0.894427190999916,0.,-0.447213595499958));
#2286=DIRECTION('',(0.894427190999916,0.,0.447213595499958));
#2287=DIRECTION('center_axis',(0.,1.,0.));
#2288=DIRECTION('ref_axis',(0.,0.,1.));
#2289=DIRECTION('center_axis',(0.,1.,0.));
#2290=DIRECTION('ref_axis',(1.,0.,0.));
#2291=DIRECTION('axis',(0.,0.,1.));
#2292=DIRECTION('refdir',(1.,0.,0.));
#2293=DIRECTION('center_axis',(0.,1.,0.));
#2294=DIRECTION('ref_axis',(-1.,0.,0.));
#2295=DIRECTION('',(-0.894427190999916,0.,-0.447213595499958));
#2296=DIRECTION('',(0.,0.,-1.));
#2297=DIRECTION('',(1.,0.,0.));
#2298=DIRECTION('',(0.,0.,-1.));
#2299=DIRECTION('center_axis',(0.,-1.,0.));
#2300=DIRECTION('ref_axis',(1.,0.,0.));
#2301=DIRECTION('',(0.894427190999916,0.,0.447213595499958));
#2302=DIRECTION('',(0.,0.,-1.));
#2303=DIRECTION('',(-1.,0.,0.));
#2304=DIRECTION('',(0.,0.,1.));
#2305=DIRECTION('center_axis',(0.,0.,1.));
#2306=DIRECTION('ref_axis',(1.,0.,0.));
#2307=DIRECTION('',(-1.,0.,0.));
#2308=DIRECTION('',(0.,1.,0.));
#2309=DIRECTION('',(1.,0.,0.));
#2310=DIRECTION('',(0.,1.,0.));
#2311=DIRECTION('center_axis',(0.,0.,-1.));
#2312=DIRECTION('ref_axis',(1.,0.,0.));
#2313=DIRECTION('center_axis',(0.,0.,-1.));
#2314=DIRECTION('ref_axis',(1.,0.,0.));
#2315=DIRECTION('center_axis',(0.,0.,1.));
#2316=DIRECTION('ref_axis',(-1.,1.22464679914735E-16,0.));
#2317=DIRECTION('center_axis',(-0.447213595499958,0.,0.894427190999916));
#2318=DIRECTION('ref_axis',(0.894427190999916,0.,0.447213595499958));
#2319=DIRECTION('center_axis',(0.,0.,1.));
#2320=DIRECTION('ref_axis',(1.,0.,0.));
#2321=DIRECTION('center_axis',(-0.447213595499958,0.,0.894427190999916));
#2322=DIRECTION('ref_axis',(0.894427190999916,0.,0.447213595499958));
#2323=DIRECTION('center_axis',(-1.,0.,0.));
#2324=DIRECTION('ref_axis',(0.,0.,1.));
#2325=DIRECTION('',(0.,0.,-1.));
#2326=DIRECTION('',(0.,0.,1.));
#2327=DIRECTION('',(0.,1.,0.));
#2328=DIRECTION('center_axis',(0.447213595499958,0.,-0.894427190999916));
#2329=DIRECTION('ref_axis',(-0.894427190999916,0.,-0.447213595499958));
#2330=DIRECTION('',(0.894427190999916,0.,0.447213595499958));
#2331=DIRECTION('',(-0.894427190999916,0.,-0.447213595499958));
#2332=DIRECTION('',(0.,1.,0.));
#2333=DIRECTION('center_axis',(1.,0.,0.));
#2334=DIRECTION('ref_axis',(0.,0.,-1.));
#2335=DIRECTION('',(0.,0.,1.));
#2336=DIRECTION('',(0.,0.,-1.));
#2337=DIRECTION('center_axis',(0.,1.,0.));
#2338=DIRECTION('ref_axis',(0.,0.,1.));
#2339=DIRECTION('center_axis',(0.,1.,0.));
#2340=DIRECTION('ref_axis',(1.,0.,0.));
#2341=DIRECTION('axis',(0.,0.,1.));
#2342=DIRECTION('refdir',(1.,0.,0.));
#2343=DIRECTION('center_axis',(0.866025403784439,0.,-0.5));
#2344=DIRECTION('ref_axis',(0.5,0.,0.866025403784439));
#2345=DIRECTION('',(-0.5,0.,-0.866025403784439));
#2346=DIRECTION('',(0.,-1.,0.));
#2347=DIRECTION('',(0.5,0.,0.866025403784439));
#2348=DIRECTION('',(0.,-1.,0.));
#2349=DIRECTION('center_axis',(1.20185167898973E-16,0.,-1.));
#2350=DIRECTION('ref_axis',(1.,0.,1.20185167898973E-16));
#2351=DIRECTION('',(-1.,0.,-1.20185167898973E-16));
#2352=DIRECTION('',(0.,-1.,0.));
#2353=DIRECTION('',(1.,0.,1.20185167898973E-16));
#2354=DIRECTION('center_axis',(-0.866025403784439,0.,-0.5));
#2355=DIRECTION('ref_axis',(0.5,0.,-0.866025403784439));
#2356=DIRECTION('',(-0.5,0.,0.866025403784439));
#2357=DIRECTION('',(0.,-1.,0.));
#2358=DIRECTION('',(0.5,0.,-0.866025403784439));
#2359=DIRECTION('center_axis',(-0.866025403784439,0.,0.5));
#2360=DIRECTION('ref_axis',(-0.5,0.,-0.866025403784439));
#2361=DIRECTION('',(0.5,0.,0.866025403784439));
#2362=DIRECTION('',(0.,-1.,0.));
#2363=DIRECTION('',(-0.5,0.,-0.866025403784439));
#2364=DIRECTION('center_axis',(-2.40370335797945E-16,0.,1.));
#2365=DIRECTION('ref_axis',(-1.,0.,-2.40370335797945E-16));
#2366=DIRECTION('',(1.,0.,2.40370335797945E-16));
#2367=DIRECTION('',(0.,-1.,0.));
#2368=DIRECTION('',(-1.,0.,-2.40370335797945E-16));
#2369=DIRECTION('center_axis',(0.866025403784439,0.,0.5));
#2370=DIRECTION('ref_axis',(-0.5,0.,0.866025403784439));
#2371=DIRECTION('',(0.5,0.,-0.866025403784439));
#2372=DIRECTION('',(-0.5,0.,0.866025403784439));
#2373=DIRECTION('center_axis',(0.,1.,0.));
#2374=DIRECTION('ref_axis',(1.,0.,0.));
#2375=DIRECTION('center_axis',(0.,-1.,0.));
#2376=DIRECTION('ref_axis',(0.,0.,-1.));
#2377=DIRECTION('center_axis',(0.,1.,0.));
#2378=DIRECTION('ref_axis',(1.,0.,0.));
#2379=DIRECTION('center_axis',(0.,1.,0.));
#2380=DIRECTION('ref_axis',(1.,0.,0.));
#2381=DIRECTION('center_axis',(0.,1.,0.));
#2382=DIRECTION('ref_axis',(0.,0.,1.));
#2383=DIRECTION('center_axis',(0.,-1.,0.));
#2384=DIRECTION('ref_axis',(1.,0.,0.));
#2385=DIRECTION('center_axis',(0.,-1.,0.));
#2386=DIRECTION('ref_axis',(1.,0.,0.));
#2387=DIRECTION('center_axis',(0.,-1.,0.));
#2388=DIRECTION('ref_axis',(1.,0.,0.));
#2389=DIRECTION('',(0.707106781186548,0.707106781186547,8.65956056235493E-17));
#2390=DIRECTION('center_axis',(0.,-1.,0.));
#2391=DIRECTION('ref_axis',(1.,0.,0.));
#2392=DIRECTION('center_axis',(0.,-1.,0.));
#2393=DIRECTION('ref_axis',(1.,0.,0.));
#2394=DIRECTION('',(0.,1.,0.));
#2395=DIRECTION('center_axis',(0.,1.,0.));
#2396=DIRECTION('ref_axis',(1.,0.,0.));
#2397=DIRECTION('center_axis',(0.,-1.,0.));
#2398=DIRECTION('ref_axis',(1.,0.,0.));
#2399=DIRECTION('',(-0.707106781186547,0.707106781186548,-8.65956056235493E-17));
#2400=DIRECTION('center_axis',(0.,-1.,0.));
#2401=DIRECTION('ref_axis',(0.,0.,-1.));
#2402=DIRECTION('center_axis',(0.,-1.,0.));
#2403=DIRECTION('ref_axis',(1.,0.,0.));
#2404=DIRECTION('center_axis',(0.,1.,0.));
#2405=DIRECTION('ref_axis',(1.,0.,0.));
#2406=DIRECTION('center_axis',(0.,1.,0.));
#2407=DIRECTION('ref_axis',(1.,0.,0.));
#2408=DIRECTION('',(-0.447213595499958,0.894427190999916,-5.47678698264203E-17));
#2409=DIRECTION('center_axis',(0.,-1.,0.));
#2410=DIRECTION('ref_axis',(1.,0.,0.));
#2411=DIRECTION('',(0.,1.,0.));
#2412=DIRECTION('axis',(0.,0.,1.));
#2413=DIRECTION('refdir',(1.,0.,0.));
#2414=DIRECTION('center_axis',(0.,1.,0.));
#2415=DIRECTION('ref_axis',(1.,0.,0.));
#2416=DIRECTION('center_axis',(0.,-1.,0.));
#2417=DIRECTION('ref_axis',(1.,0.,0.));
#2418=DIRECTION('',(0.,-1.,0.));
#2419=DIRECTION('center_axis',(0.,-1.,0.));
#2420=DIRECTION('ref_axis',(1.,0.,0.));
#2421=DIRECTION('center_axis',(0.,1.,0.));
#2422=DIRECTION('ref_axis',(1.,0.,0.));
#2423=DIRECTION('center_axis',(0.,1.,0.));
#2424=DIRECTION('ref_axis',(1.,0.,0.));
#2425=DIRECTION('',(0.,-1.,0.));
#2426=DIRECTION('center_axis',(0.,1.,0.));
#2427=DIRECTION('ref_axis',(1.,0.,0.));
#2428=DIRECTION('center_axis',(0.,1.,0.));
#2429=DIRECTION('ref_axis',(1.,0.,0.));
#2430=DIRECTION('center_axis',(0.,1.,0.));
#2431=DIRECTION('ref_axis',(1.,0.,0.));
#2432=DIRECTION('axis',(0.,0.,1.));
#2433=DIRECTION('refdir',(1.,0.,0.));
#2434=DIRECTION('center_axis',(0.,-1.,0.));
#2435=DIRECTION('ref_axis',(1.,0.,0.));
#2436=DIRECTION('center_axis',(0.,1.,0.));
#2437=DIRECTION('ref_axis',(1.,0.,0.));
#2438=DIRECTION('',(0.,1.,0.));
#2439=DIRECTION('center_axis',(0.,-1.,0.));
#2440=DIRECTION('ref_axis',(1.,0.,0.));
#2441=DIRECTION('center_axis',(0.,1.,0.));
#2442=DIRECTION('ref_axis',(1.,0.,0.));
#2443=DIRECTION('center_axis',(0.,-1.,0.));
#2444=DIRECTION('ref_axis',(1.,0.,0.));
#2445=DIRECTION('',(-0.707106781186549,0.707106781186546,-8.65956056235496E-17));
#2446=DIRECTION('center_axis',(0.,-1.,0.));
#2447=DIRECTION('ref_axis',(0.,0.,-1.));
#2448=DIRECTION('center_axis',(0.,-1.,0.));
#2449=DIRECTION('ref_axis',(1.,0.,0.));
#2450=DIRECTION('center_axis',(0.,1.,0.));
#2451=DIRECTION('ref_axis',(1.,0.,0.));
#2452=DIRECTION('',(-0.866025403784439,-0.5,-1.06057523872491E-16));
#2453=DIRECTION('center_axis',(1.4792020664489E-16,0.,-1.));
#2454=DIRECTION('ref_axis',(-1.,0.,-1.4792020664489E-16));
#2455=DIRECTION('',(0.,1.,0.));
#2456=DIRECTION('',(-1.,0.,-1.4792020664489E-16));
#2457=DIRECTION('',(0.,1.,0.));
#2458=DIRECTION('center_axis',(0.866025403784439,0.,-0.5));
#2459=DIRECTION('ref_axis',(-0.5,0.,-0.866025403784439));
#2460=DIRECTION('',(0.,1.,0.));
#2461=DIRECTION('',(-0.5,0.,-0.866025403784439));
#2462=DIRECTION('center_axis',(0.866025403784439,0.,0.5));
#2463=DIRECTION('ref_axis',(0.5,0.,-0.866025403784439));
#2464=DIRECTION('',(0.,1.,0.));
#2465=DIRECTION('',(0.5,0.,-0.866025403784439));
#2466=DIRECTION('center_axis',(-2.95840413289779E-16,0.,1.));
#2467=DIRECTION('ref_axis',(1.,0.,2.95840413289779E-16));
#2468=DIRECTION('',(0.,1.,0.));
#2469=DIRECTION('',(1.,0.,2.95840413289779E-16));
#2470=DIRECTION('center_axis',(-0.866025403784439,0.,0.5));
#2471=DIRECTION('ref_axis',(0.5,0.,0.866025403784439));
#2472=DIRECTION('',(0.,1.,0.));
#2473=DIRECTION('',(0.5,0.,0.866025403784439));
#2474=DIRECTION('center_axis',(-0.866025403784439,0.,-0.5));
#2475=DIRECTION('ref_axis',(-0.5,0.,0.866025403784439));
#2476=DIRECTION('',(-0.5,0.,0.866025403784439));
#2477=DIRECTION('center_axis',(0.,1.,0.));
#2478=DIRECTION('ref_axis',(0.,0.,1.));
#2479=DIRECTION('center_axis',(0.,1.,0.));
#2480=DIRECTION('ref_axis',(1.,0.,0.));
#2481=DIRECTION('',(0.,0.,1.));
#2482=DIRECTION('',(1.,0.,0.));
#2483=DIRECTION('',(0.,0.,1.));
#2484=DIRECTION('',(1.,0.,0.));
#2485=DIRECTION('',(0.,0.,1.));
#2486=DIRECTION('',(1.,0.,0.));
#2487=DIRECTION('',(0.,1.,2.22044604925031E-16));
#2488=DIRECTION('',(1.,0.,0.));
#2489=DIRECTION('',(0.,1.,2.22044604925031E-16));
#2490=DIRECTION('',(1.,0.,0.));
#2491=DIRECTION('',(0.,1.,2.22044604925031E-16));
#2492=DIRECTION('',(1.,0.,0.));
#2493=DIRECTION('',(0.,1.,2.22044604925031E-16));
#2494=DIRECTION('',(1.,0.,0.));
#2495=DIRECTION('',(0.,-1.,2.22044604925031E-16));
#2496=DIRECTION('',(1.,0.,0.));
#2497=DIRECTION('',(0.,-1.,2.22044604925031E-16));
#2498=DIRECTION('',(1.,0.,0.));
#2499=DIRECTION('',(0.,0.,1.));
#2500=DIRECTION('',(1.,0.,0.));
#2501=CARTESIAN_POINT('',(0.,0.,0.));
#2502=CARTESIAN_POINT('',(0.,0.,0.));
#2503=CARTESIAN_POINT('',(0.,0.,0.));
#2504=CARTESIAN_POINT('Origin',(2.5,-1.5,-0.1));
#2505=CARTESIAN_POINT('',(2.225,-1.5,0.));
#2506=CARTESIAN_POINT('Origin',(2.5,-1.5,0.));
#2507=CARTESIAN_POINT('',(2.225,-1.5,1.));
#2508=CARTESIAN_POINT('',(2.225,-1.5,-0.1));
#2509=CARTESIAN_POINT('Origin',(2.5,-1.5,1.));
#2510=CARTESIAN_POINT('Origin',(0.5,1.5,-0.1));
#2511=CARTESIAN_POINT('',(0.225,1.5,0.));
#2512=CARTESIAN_POINT('Origin',(0.5,1.5,0.));
#2513=CARTESIAN_POINT('',(0.225,1.5,1.));
#2514=CARTESIAN_POINT('',(0.225,1.5,-0.1));
#2515=CARTESIAN_POINT('Origin',(0.5,1.5,1.));
#2516=CARTESIAN_POINT('Origin',(0.5,-1.5,-0.1));
#2517=CARTESIAN_POINT('',(0.225,-1.5,0.));
#2518=CARTESIAN_POINT('Origin',(0.5,-1.5,0.));
#2519=CARTESIAN_POINT('',(0.225,-1.5,1.));
#2520=CARTESIAN_POINT('',(0.225,-1.5,-0.1));
#2521=CARTESIAN_POINT('Origin',(0.5,-1.5,1.));
#2522=CARTESIAN_POINT('Origin',(2.5,1.5,-0.1));
#2523=CARTESIAN_POINT('',(2.225,1.5,0.));
#2524=CARTESIAN_POINT('Origin',(2.5,1.5,0.));
#2525=CARTESIAN_POINT('',(2.225,1.5,1.));
#2526=CARTESIAN_POINT('',(2.225,1.5,-0.1));
#2527=CARTESIAN_POINT('Origin',(2.5,1.5,1.));
#2528=CARTESIAN_POINT('Origin',(1.5,0.,-0.1));
#2529=CARTESIAN_POINT('',(1.16,-4.163799117101E-17,0.));
#2530=CARTESIAN_POINT('Origin',(1.5,0.,0.));
#2531=CARTESIAN_POINT('',(1.16,4.163799117101E-17,1.));
#2532=CARTESIAN_POINT('',(1.16,-4.163799117101E-17,-0.1));
#2533=CARTESIAN_POINT('Origin',(1.5,0.,1.));
#2534=CARTESIAN_POINT('Origin',(5.,2.5,-0.1));
#2535=CARTESIAN_POINT('',(4.66,2.5,0.));
#2536=CARTESIAN_POINT('Origin',(5.,2.5,0.));
#2537=CARTESIAN_POINT('',(4.66,2.5,1.));
#2538=CARTESIAN_POINT('',(4.66,2.5,-0.1));
#2539=CARTESIAN_POINT('Origin',(5.,2.5,1.));
#2540=CARTESIAN_POINT('Origin',(5.,-2.5,-0.1));
#2541=CARTESIAN_POINT('',(4.66,-2.5,0.));
#2542=CARTESIAN_POINT('Origin',(5.,-2.5,0.));
#2543=CARTESIAN_POINT('',(4.66,-2.5,1.));
#2544=CARTESIAN_POINT('',(4.66,-2.5,-0.1));
#2545=CARTESIAN_POINT('Origin',(5.,-2.5,1.));
#2546=CARTESIAN_POINT('Origin',(2.5,5.,-0.1));
#2547=CARTESIAN_POINT('',(2.16,5.,0.));
#2548=CARTESIAN_POINT('Origin',(2.5,5.,0.));
#2549=CARTESIAN_POINT('',(2.16,5.,1.));
#2550=CARTESIAN_POINT('',(2.16,5.,-0.1));
#2551=CARTESIAN_POINT('Origin',(2.5,5.,1.));
#2552=CARTESIAN_POINT('Origin',(2.5,0.,-0.1));
#2553=CARTESIAN_POINT('',(2.16,-4.163799117101E-17,0.));
#2554=CARTESIAN_POINT('Origin',(2.5,0.,0.));
#2555=CARTESIAN_POINT('',(2.16,4.163799117101E-17,1.));
#2556=CARTESIAN_POINT('',(2.16,-4.163799117101E-17,-0.1));
#2557=CARTESIAN_POINT('Origin',(2.5,0.,1.));
#2558=CARTESIAN_POINT('Origin',(2.5,-5.,-0.1));
#2559=CARTESIAN_POINT('',(2.16,-5.,0.));
#2560=CARTESIAN_POINT('Origin',(2.5,-5.,0.));
#2561=CARTESIAN_POINT('',(2.16,-5.,1.));
#2562=CARTESIAN_POINT('',(2.16,-5.,-0.1));
#2563=CARTESIAN_POINT('Origin',(2.5,-5.,1.));
#2564=CARTESIAN_POINT('Origin',(0.,2.5,-0.1));
#2565=CARTESIAN_POINT('',(-0.34,2.5,0.));
#2566=CARTESIAN_POINT('Origin',(0.,2.5,0.));
#2567=CARTESIAN_POINT('',(-0.34,2.5,1.));
#2568=CARTESIAN_POINT('',(-0.34,2.5,-0.1));
#2569=CARTESIAN_POINT('Origin',(0.,2.5,1.));
#2570=CARTESIAN_POINT('Origin',(0.,0.,-0.1));
#2571=CARTESIAN_POINT('',(-0.34,-4.163799117101E-17,0.));
#2572=CARTESIAN_POINT('Origin',(0.,0.,0.));
#2573=CARTESIAN_POINT('',(-0.34,4.163799117101E-17,1.));
#2574=CARTESIAN_POINT('',(-0.34,-4.163799117101E-17,-0.1));
#2575=CARTESIAN_POINT('Origin',(0.,0.,1.));
#2576=CARTESIAN_POINT('Origin',(0.,-5.,-0.1));
#2577=CARTESIAN_POINT('',(-0.34,-5.,0.));
#2578=CARTESIAN_POINT('Origin',(0.,-5.,0.));
#2579=CARTESIAN_POINT('',(-0.34,-5.,1.));
#2580=CARTESIAN_POINT('',(-0.34,-5.,-0.1));
#2581=CARTESIAN_POINT('Origin',(0.,-5.,1.));
#2582=CARTESIAN_POINT('Origin',(-2.5,2.5,-0.1));
#2583=CARTESIAN_POINT('',(-2.84,2.5,0.));
#2584=CARTESIAN_POINT('Origin',(-2.5,2.5,0.));
#2585=CARTESIAN_POINT('',(-2.84,2.5,1.));
#2586=CARTESIAN_POINT('',(-2.84,2.5,-0.1));
#2587=CARTESIAN_POINT('Origin',(-2.5,2.5,1.));
#2588=CARTESIAN_POINT('Origin',(-2.5,-2.5,-0.1));
#2589=CARTESIAN_POINT('',(-2.84,-2.5,0.));
#2590=CARTESIAN_POINT('Origin',(-2.5,-2.5,0.));
#2591=CARTESIAN_POINT('',(-2.84,-2.5,1.));
#2592=CARTESIAN_POINT('',(-2.84,-2.5,-0.1));
#2593=CARTESIAN_POINT('Origin',(-2.5,-2.5,1.));
#2594=CARTESIAN_POINT('Origin',(-5.,5.,-0.1));
#2595=CARTESIAN_POINT('',(-5.34,5.,0.));
#2596=CARTESIAN_POINT('Origin',(-5.,5.,0.));
#2597=CARTESIAN_POINT('',(-5.34,5.,1.));
#2598=CARTESIAN_POINT('',(-5.34,5.,-0.1));
#2599=CARTESIAN_POINT('Origin',(-5.,5.,1.));
#2600=CARTESIAN_POINT('Origin',(-5.,0.,-0.1));
#2601=CARTESIAN_POINT('',(-5.34,-4.163799117101E-17,0.));
#2602=CARTESIAN_POINT('Origin',(-5.,0.,0.));
#2603=CARTESIAN_POINT('',(-5.34,4.163799117101E-17,1.));
#2604=CARTESIAN_POINT('',(-5.34,-4.163799117101E-17,-0.1));
#2605=CARTESIAN_POINT('Origin',(-5.,0.,1.));
#2606=CARTESIAN_POINT('Origin',(-5.,-2.5,-0.1));
#2607=CARTESIAN_POINT('',(-5.34,-2.5,0.));
#2608=CARTESIAN_POINT('Origin',(-5.,-2.5,0.));
#2609=CARTESIAN_POINT('',(-5.34,-2.5,1.));
#2610=CARTESIAN_POINT('',(-5.34,-2.5,-0.1));
#2611=CARTESIAN_POINT('Origin',(-5.,-2.5,1.));
#2612=CARTESIAN_POINT('Origin',(-5.,2.5,-0.1));
#2613=CARTESIAN_POINT('',(-5.34,2.5,0.));
#2614=CARTESIAN_POINT('Origin',(-5.,2.5,0.));
#2615=CARTESIAN_POINT('',(-5.34,2.5,1.));
#2616=CARTESIAN_POINT('',(-5.34,2.5,-0.1));
#2617=CARTESIAN_POINT('Origin',(-5.,2.5,1.));
#2618=CARTESIAN_POINT('Origin',(-2.5,-5.,-0.1));
#2619=CARTESIAN_POINT('',(-2.84,-5.,0.));
#2620=CARTESIAN_POINT('Origin',(-2.5,-5.,0.));
#2621=CARTESIAN_POINT('',(-2.84,-5.,1.));
#2622=CARTESIAN_POINT('',(-2.84,-5.,-0.1));
#2623=CARTESIAN_POINT('Origin',(-2.5,-5.,1.));
#2624=CARTESIAN_POINT('Origin',(-2.5,0.,-0.1));
#2625=CARTESIAN_POINT('',(-2.84,-4.163799117101E-17,0.));
#2626=CARTESIAN_POINT('Origin',(-2.5,0.,0.));
#2627=CARTESIAN_POINT('',(-2.84,4.163799117101E-17,1.));
#2628=CARTESIAN_POINT('',(-2.84,-4.163799117101E-17,-0.1));
#2629=CARTESIAN_POINT('Origin',(-2.5,0.,1.));
#2630=CARTESIAN_POINT('Origin',(-2.5,5.,-0.1));
#2631=CARTESIAN_POINT('',(-2.84,5.,0.));
#2632=CARTESIAN_POINT('Origin',(-2.5,5.,0.));
#2633=CARTESIAN_POINT('',(-2.84,5.,1.));
#2634=CARTESIAN_POINT('',(-2.84,5.,-0.1));
#2635=CARTESIAN_POINT('Origin',(-2.5,5.,1.));
#2636=CARTESIAN_POINT('Origin',(0.,-2.5,-0.1));
#2637=CARTESIAN_POINT('',(-0.34,-2.5,0.));
#2638=CARTESIAN_POINT('Origin',(0.,-2.5,0.));
#2639=CARTESIAN_POINT('',(-0.34,-2.5,1.));
#2640=CARTESIAN_POINT('',(-0.34,-2.5,-0.1));
#2641=CARTESIAN_POINT('Origin',(0.,-2.5,1.));
#2642=CARTESIAN_POINT('Origin',(-5.,-5.,-0.1));
#2643=CARTESIAN_POINT('',(-5.34,-5.,0.));
#2644=CARTESIAN_POINT('Origin',(-5.,-5.,0.));
#2645=CARTESIAN_POINT('',(-5.34,-5.,1.));
#2646=CARTESIAN_POINT('',(-5.34,-5.,-0.1));
#2647=CARTESIAN_POINT('Origin',(-5.,-5.,1.));
#2648=CARTESIAN_POINT('Origin',(0.,5.,-0.1));
#2649=CARTESIAN_POINT('',(-0.34,5.,0.));
#2650=CARTESIAN_POINT('Origin',(0.,5.,0.));
#2651=CARTESIAN_POINT('',(-0.34,5.,1.));
#2652=CARTESIAN_POINT('',(-0.34,5.,-0.1));
#2653=CARTESIAN_POINT('Origin',(0.,5.,1.));
#2654=CARTESIAN_POINT('Origin',(2.5,-2.5,-0.1));
#2655=CARTESIAN_POINT('',(2.16,-2.5,0.));
#2656=CARTESIAN_POINT('Origin',(2.5,-2.5,0.));
#2657=CARTESIAN_POINT('',(2.16,-2.5,1.));
#2658=CARTESIAN_POINT('',(2.16,-2.5,-0.1));
#2659=CARTESIAN_POINT('Origin',(2.5,-2.5,1.));
#2660=CARTESIAN_POINT('Origin',(2.5,2.5,-0.1));
#2661=CARTESIAN_POINT('',(2.16,2.5,0.));
#2662=CARTESIAN_POINT('Origin',(2.5,2.5,0.));
#2663=CARTESIAN_POINT('',(2.16,2.5,1.));
#2664=CARTESIAN_POINT('',(2.16,2.5,-0.1));
#2665=CARTESIAN_POINT('Origin',(2.5,2.5,1.));
#2666=CARTESIAN_POINT('Origin',(5.,-5.,-0.1));
#2667=CARTESIAN_POINT('',(4.66,-5.,0.));
#2668=CARTESIAN_POINT('Origin',(5.,-5.,0.));
#2669=CARTESIAN_POINT('',(4.66,-5.,1.));
#2670=CARTESIAN_POINT('',(4.66,-5.,-0.1));
#2671=CARTESIAN_POINT('Origin',(5.,-5.,1.));
#2672=CARTESIAN_POINT('Origin',(5.,0.,-0.1));
#2673=CARTESIAN_POINT('',(4.66,-4.163799117101E-17,0.));
#2674=CARTESIAN_POINT('Origin',(5.,0.,0.));
#2675=CARTESIAN_POINT('',(4.66,4.163799117101E-17,1.));
#2676=CARTESIAN_POINT('',(4.66,-4.163799117101E-17,-0.1));
#2677=CARTESIAN_POINT('Origin',(5.,0.,1.));
#2678=CARTESIAN_POINT('Origin',(5.,5.,-0.1));
#2679=CARTESIAN_POINT('',(4.66,5.,0.));
#2680=CARTESIAN_POINT('Origin',(5.,5.,0.));
#2681=CARTESIAN_POINT('',(4.66,5.,1.));
#2682=CARTESIAN_POINT('',(4.66,5.,-0.1));
#2683=CARTESIAN_POINT('Origin',(5.,5.,1.));
#2684=CARTESIAN_POINT('Origin',(7.5,7.5,0.));
#2685=CARTESIAN_POINT('',(7.5,7.5,0.));
#2686=CARTESIAN_POINT('',(-7.5,7.5,0.));
#2687=CARTESIAN_POINT('',(7.5,7.5,0.));
#2688=CARTESIAN_POINT('',(-7.5,7.5,1.));
#2689=CARTESIAN_POINT('',(-7.5,7.5,0.));
#2690=CARTESIAN_POINT('',(7.5,7.5,1.));
#2691=CARTESIAN_POINT('',(7.5,7.5,1.));
#2692=CARTESIAN_POINT('',(7.5,7.5,0.));
#2693=CARTESIAN_POINT('Origin',(7.5,-7.5,0.));
#2694=CARTESIAN_POINT('',(7.5,-7.5,0.));
#2695=CARTESIAN_POINT('',(7.5,-7.5,0.));
#2696=CARTESIAN_POINT('',(7.5,-7.5,1.));
#2697=CARTESIAN_POINT('',(7.5,-7.5,1.));
#2698=CARTESIAN_POINT('',(7.5,-7.5,0.));
#2699=CARTESIAN_POINT('Origin',(-7.5,-7.5,0.));
#2700=CARTESIAN_POINT('',(-7.5,-7.5,0.));
#2701=CARTESIAN_POINT('',(-7.5,-7.5,0.));
#2702=CARTESIAN_POINT('',(-7.5,-7.5,1.));
#2703=CARTESIAN_POINT('',(-7.5,-7.5,1.));
#2704=CARTESIAN_POINT('',(-7.5,-7.5,0.));
#2705=CARTESIAN_POINT('Origin',(-7.5,7.5,0.));
#2706=CARTESIAN_POINT('',(-7.5,7.5,0.));
#2707=CARTESIAN_POINT('',(-7.5,7.5,1.));
#2708=CARTESIAN_POINT('Origin',(0.,0.,1.));
#2709=CARTESIAN_POINT('Origin',(0.,0.,0.));
#2710=CARTESIAN_POINT('',(0.,0.,0.));
#2711=CARTESIAN_POINT('Origin',(2.5,-1.5,0.9));
#2712=CARTESIAN_POINT('',(2.29,-1.5,1.));
#2713=CARTESIAN_POINT('Origin',(2.5,-1.5,1.));
#2714=CARTESIAN_POINT('',(2.29,-1.5,1.5));
#2715=CARTESIAN_POINT('',(2.29,-1.5,0.9));
#2716=CARTESIAN_POINT('Origin',(2.5,-1.5,1.5));
#2717=CARTESIAN_POINT('Origin',(2.5,-1.5,1.5));
#2718=CARTESIAN_POINT('Origin',(0.5,1.5,0.9));
#2719=CARTESIAN_POINT('',(0.29,1.5,1.));
#2720=CARTESIAN_POINT('Origin',(0.5,1.5,1.));
#2721=CARTESIAN_POINT('',(0.29,1.5,1.5));
#2722=CARTESIAN_POINT('',(0.29,1.5,0.9));
#2723=CARTESIAN_POINT('Origin',(0.5,1.5,1.5));
#2724=CARTESIAN_POINT('Origin',(0.5,1.5,1.5));
#2725=CARTESIAN_POINT('Origin',(0.5,-1.5,0.9));
#2726=CARTESIAN_POINT('',(0.29,-1.5,1.));
#2727=CARTESIAN_POINT('Origin',(0.5,-1.5,1.));
#2728=CARTESIAN_POINT('',(0.29,-1.5,1.5));
#2729=CARTESIAN_POINT('',(0.29,-1.5,0.9));
#2730=CARTESIAN_POINT('Origin',(0.5,-1.5,1.5));
#2731=CARTESIAN_POINT('Origin',(0.5,-1.5,1.5));
#2732=CARTESIAN_POINT('Origin',(2.5,1.5,0.9));
#2733=CARTESIAN_POINT('',(2.29,1.5,1.));
#2734=CARTESIAN_POINT('Origin',(2.5,1.5,1.));
#2735=CARTESIAN_POINT('',(2.29,1.5,1.5));
#2736=CARTESIAN_POINT('',(2.29,1.5,0.9));
#2737=CARTESIAN_POINT('Origin',(2.5,1.5,1.5));
#2738=CARTESIAN_POINT('Origin',(2.5,1.5,1.5));
#2739=CARTESIAN_POINT('Origin',(1.5,0.,0.9));
#2740=CARTESIAN_POINT('',(1.075,-5.20474889637625E-17,1.));
#2741=CARTESIAN_POINT('Origin',(1.5,0.,1.));
#2742=CARTESIAN_POINT('',(1.075,5.20474889637625E-17,2.1375));
#2743=CARTESIAN_POINT('',(1.075,-5.20474889637625E-17,0.9));
#2744=CARTESIAN_POINT('Origin',(1.5,0.,2.35));
#2745=CARTESIAN_POINT('Origin',(0.,-2.,1.));
#2746=CARTESIAN_POINT('',(0.,-2.,1.6));
#2747=CARTESIAN_POINT('',(0.,-2.,1.));
#2748=CARTESIAN_POINT('',(0.,-2.,1.6));
#2749=CARTESIAN_POINT('',(0.,2.,1.6));
#2750=CARTESIAN_POINT('',(0.,-2.,1.6));
#2751=CARTESIAN_POINT('',(0.,2.,1.));
#2752=CARTESIAN_POINT('',(0.,2.,1.6));
#2753=CARTESIAN_POINT('',(0.,-2.,1.));
#2754=CARTESIAN_POINT('Origin',(3.,-2.,1.));
#2755=CARTESIAN_POINT('',(3.,-2.,1.));
#2756=CARTESIAN_POINT('',(0.,-2.,1.));
#2757=CARTESIAN_POINT('',(3.,2.,1.));
#2758=CARTESIAN_POINT('',(0.,2.,1.));
#2759=CARTESIAN_POINT('',(3.,-2.,1.));
#2760=CARTESIAN_POINT('Origin',(3.,-2.,3.1));
#2761=CARTESIAN_POINT('',(3.,-2.,3.1));
#2762=CARTESIAN_POINT('',(3.,-2.,1.));
#2763=CARTESIAN_POINT('',(3.,2.,3.1));
#2764=CARTESIAN_POINT('',(3.,2.,1.));
#2765=CARTESIAN_POINT('',(3.,-2.,3.1));
#2766=CARTESIAN_POINT('Origin',(0.,-2.,1.6));
#2767=CARTESIAN_POINT('',(3.,-2.,3.1));
#2768=CARTESIAN_POINT('',(3.,2.,3.1));
#2769=CARTESIAN_POINT('Origin',(1.5,2.,2.05));
#2770=CARTESIAN_POINT('Origin',(1.5,-2.,2.05));
#2771=CARTESIAN_POINT('',(0.,0.,0.));
#2772=CARTESIAN_POINT('Origin',(2.05,0.45,1.5));
#2773=CARTESIAN_POINT('',(2.05,0.45,2.625));
#2774=CARTESIAN_POINT('',(0.95,0.45,2.075));
#2775=CARTESIAN_POINT('',(2.3,0.45,2.75));
#2776=CARTESIAN_POINT('',(2.05,0.45,4.));
#2777=CARTESIAN_POINT('',(2.05,0.45,1.5));
#2778=CARTESIAN_POINT('',(0.95,0.45,4.));
#2779=CARTESIAN_POINT('',(1.025,0.45,4.));
#2780=CARTESIAN_POINT('',(0.95,0.45,1.5));
#2781=CARTESIAN_POINT('Origin',(0.95,-0.45,1.5));
#2782=CARTESIAN_POINT('',(0.95,-0.45,2.075));
#2783=CARTESIAN_POINT('',(2.05,-0.45,2.625));
#2784=CARTESIAN_POINT('',(1.86,-0.45,2.53));
#2785=CARTESIAN_POINT('',(0.95,-0.45,4.));
#2786=CARTESIAN_POINT('',(0.95,-0.45,1.5));
#2787=CARTESIAN_POINT('',(2.05,-0.45,4.));
#2788=CARTESIAN_POINT('',(0.475,-0.45,4.));
#2789=CARTESIAN_POINT('',(2.05,-0.45,1.5));
#2790=CARTESIAN_POINT('Origin',(0.,-2.,4.));
#2791=CARTESIAN_POINT('',(3.,-2.,4.));
#2792=CARTESIAN_POINT('',(0.,-2.,4.));
#2793=CARTESIAN_POINT('',(3.,-2.,4.));
#2794=CARTESIAN_POINT('',(3.,2.,4.));
#2795=CARTESIAN_POINT('',(3.,-2.,4.));
#2796=CARTESIAN_POINT('',(0.,2.,4.));
#2797=CARTESIAN_POINT('',(3.,2.,4.));
#2798=CARTESIAN_POINT('',(0.,-2.,4.));
#2799=CARTESIAN_POINT('Origin',(2.05,0.,4.));
#2800=CARTESIAN_POINT('Origin',(0.95,0.,4.));
#2801=CARTESIAN_POINT('Origin',(0.95,0.,1.5));
#2802=CARTESIAN_POINT('Origin',(0.95,0.,2.075));
#2803=CARTESIAN_POINT('Origin',(2.05,0.,1.5));
#2804=CARTESIAN_POINT('Origin',(2.05,0.,2.625));
#2805=CARTESIAN_POINT('Origin',(0.,-2.,1.6));
#2806=CARTESIAN_POINT('',(0.,-2.,1.6));
#2807=CARTESIAN_POINT('',(0.,-2.,4.));
#2808=CARTESIAN_POINT('',(0.,2.,1.6));
#2809=CARTESIAN_POINT('',(0.,2.,4.));
#2810=CARTESIAN_POINT('',(0.,-2.,1.6));
#2811=CARTESIAN_POINT('Origin',(3.,-2.,3.1));
#2812=CARTESIAN_POINT('',(3.,-2.,3.1));
#2813=CARTESIAN_POINT('',(0.,-2.,1.6));
#2814=CARTESIAN_POINT('',(3.,2.,3.1));
#2815=CARTESIAN_POINT('',(0.,2.,1.6));
#2816=CARTESIAN_POINT('',(3.,-2.,3.1));
#2817=CARTESIAN_POINT('Origin',(3.,-2.,4.));
#2818=CARTESIAN_POINT('',(3.,-2.,3.1));
#2819=CARTESIAN_POINT('',(3.,2.,3.1));
#2820=CARTESIAN_POINT('Origin',(1.5,2.,2.8));
#2821=CARTESIAN_POINT('Origin',(1.5,-2.,2.8));
#2822=CARTESIAN_POINT('',(0.,0.,0.));
#2823=CARTESIAN_POINT('Origin',(0.115470053837925,-0.5,-0.2));
#2824=CARTESIAN_POINT('',(0.23094010767585,-0.5,0.));
#2825=CARTESIAN_POINT('',(0.115470053837925,-0.5,-0.2));
#2826=CARTESIAN_POINT('',(0.23094010767585,-0.5,0.));
#2827=CARTESIAN_POINT('',(0.115470053837925,-0.8,-0.2));
#2828=CARTESIAN_POINT('',(0.115470053837925,-0.5,-0.2));
#2829=CARTESIAN_POINT('',(0.23094010767585,-0.8,0.));
#2830=CARTESIAN_POINT('',(0.23094010767585,-0.8,0.));
#2831=CARTESIAN_POINT('',(0.23094010767585,-0.5,0.));
#2832=CARTESIAN_POINT('Origin',(-0.115470053837925,-0.5,-0.2));
#2833=CARTESIAN_POINT('',(-0.115470053837925,-0.5,-0.2));
#2834=CARTESIAN_POINT('',(0.115470053837925,-0.5,-0.2));
#2835=CARTESIAN_POINT('',(-0.115470053837925,-0.8,-0.2));
#2836=CARTESIAN_POINT('',(-0.115470053837925,-0.5,-0.2));
#2837=CARTESIAN_POINT('',(0.115470053837925,-0.8,-0.2));
#2838=CARTESIAN_POINT('Origin',(-0.23094010767585,-0.5,-2.77555756156289E-17));
#2839=CARTESIAN_POINT('',(-0.23094010767585,-0.5,-2.82820063659975E-17));
#2840=CARTESIAN_POINT('',(-0.115470053837925,-0.5,-0.2));
#2841=CARTESIAN_POINT('',(-0.23094010767585,-0.8,-2.77555756156289E-17));
#2842=CARTESIAN_POINT('',(-0.23094010767585,-0.5,-2.82820063659975E-17));
#2843=CARTESIAN_POINT('',(-0.115470053837925,-0.8,-0.2));
#2844=CARTESIAN_POINT('Origin',(-0.115470053837925,-0.5,0.2));
#2845=CARTESIAN_POINT('',(-0.115470053837925,-0.5,0.2));
#2846=CARTESIAN_POINT('',(-0.23094010767585,-0.5,-2.82820063659975E-17));
#2847=CARTESIAN_POINT('',(-0.115470053837925,-0.8,0.2));
#2848=CARTESIAN_POINT('',(-0.115470053837925,-0.5,0.2));
#2849=CARTESIAN_POINT('',(-0.23094010767585,-0.8,-2.82820063659975E-17));
#2850=CARTESIAN_POINT('Origin',(0.115470053837925,-0.5,0.2));
#2851=CARTESIAN_POINT('',(0.115470053837925,-0.5,0.2));
#2852=CARTESIAN_POINT('',(-0.115470053837925,-0.5,0.2));
#2853=CARTESIAN_POINT('',(0.115470053837925,-0.8,0.2));
#2854=CARTESIAN_POINT('',(0.115470053837925,-0.5,0.2));
#2855=CARTESIAN_POINT('',(-0.115470053837925,-0.8,0.2));
#2856=CARTESIAN_POINT('Origin',(0.23094010767585,-0.5,0.));
#2857=CARTESIAN_POINT('',(0.115470053837925,-0.5,0.2));
#2858=CARTESIAN_POINT('',(0.115470053837925,-0.8,0.2));
#2859=CARTESIAN_POINT('Origin',(0.,-0.5,0.));
#2860=CARTESIAN_POINT('Origin',(0.,-0.8,0.));
#2861=CARTESIAN_POINT('Origin',(0.,-1.4,0.));
#2862=CARTESIAN_POINT('',(-0.24505,-1.4,3.00099698131059E-17));
#2863=CARTESIAN_POINT('Origin',(0.,-1.4,0.));
#2864=CARTESIAN_POINT('Origin',(0.375,0.5,0.));
#2865=CARTESIAN_POINT('',(-0.375,0.5,-4.59242549680257E-17));
#2866=CARTESIAN_POINT('Origin',(0.,0.5,0.));
#2867=CARTESIAN_POINT('Origin',(0.,0.475,0.));
#2868=CARTESIAN_POINT('',(-0.425,0.45,-5.20474889637625E-17));
#2869=CARTESIAN_POINT('Origin',(0.,0.45,0.));
#2870=CARTESIAN_POINT('',(-0.4,0.475,-4.89858719658941E-17));
#2871=CARTESIAN_POINT('Origin',(0.,0.24,0.));
#2872=CARTESIAN_POINT('',(-0.425,0.0299999999999998,-5.20474889637625E-17));
#2873=CARTESIAN_POINT('Origin',(0.,0.0299999999999998,0.));
#2874=CARTESIAN_POINT('',(-0.425,0.24,-5.20474889637625E-17));
#2875=CARTESIAN_POINT('Origin',(0.,0.0150000000000001,0.));
#2876=CARTESIAN_POINT('',(-0.395,4.85722573273506E-17,-4.83735485663204E-17));
#2877=CARTESIAN_POINT('Origin',(0.,0.,0.));
#2878=CARTESIAN_POINT('',(-0.41,0.0150000000000001,-5.02105187650415E-17));
#2879=CARTESIAN_POINT('Origin',(0.27,0.,0.));
#2880=CARTESIAN_POINT('',(-0.27,0.,-3.30654635769785E-17));
#2881=CARTESIAN_POINT('Origin',(0.,0.,0.));
#2882=CARTESIAN_POINT('Origin',(0.,-0.02,0.));
#2883=CARTESIAN_POINT('',(-0.24505,-0.0498999999999999,3.00099698131059E-17));
#2884=CARTESIAN_POINT('Origin',(0.,-0.0498999999999999,0.));
#2885=CARTESIAN_POINT('',(-0.26,-0.02,-3.18408167778312E-17));
#2886=CARTESIAN_POINT('Origin',(0.,-0.995,0.));
#2887=CARTESIAN_POINT('',(-0.24505,-0.995,-3.00099698131059E-17));
#2888=CARTESIAN_POINT('',(0.,0.,0.));
#2889=CARTESIAN_POINT('Origin',(0.,0.,0.));
#2890=CARTESIAN_POINT('',(-0.42,0.16,5.14351655641888E-17));
#2891=CARTESIAN_POINT('Origin',(0.,0.16,0.));
#2892=CARTESIAN_POINT('',(-0.42,0.,5.14351655641888E-17));
#2893=CARTESIAN_POINT('',(-0.42,0.,5.14351655641888E-17));
#2894=CARTESIAN_POINT('Origin',(0.,0.,0.));
#2895=CARTESIAN_POINT('Origin',(0.,0.,0.));
#2896=CARTESIAN_POINT('',(-0.8,0.16,9.79717439317883E-17));
#2897=CARTESIAN_POINT('Origin',(0.,0.16,0.));
#2898=CARTESIAN_POINT('',(-0.8,0.,9.79717439317883E-17));
#2899=CARTESIAN_POINT('',(-0.8,0.,9.79717439317883E-17));
#2900=CARTESIAN_POINT('Origin',(0.,0.,0.));
#2901=CARTESIAN_POINT('Origin',(0.,0.16,0.));
#2902=CARTESIAN_POINT('Origin',(0.,0.,0.));
#2903=CARTESIAN_POINT('',(0.,0.,0.));
#2904=CARTESIAN_POINT('Origin',(0.,-1.935,0.));
#2905=CARTESIAN_POINT('',(-0.3933,-3.9267,4.81653586104654E-17));
#2906=CARTESIAN_POINT('Origin',(0.,-3.9267,0.));
#2907=CARTESIAN_POINT('',(-0.3933,0.,-4.81653586104654E-17));
#2908=CARTESIAN_POINT('',(-0.3933,-1.935,-4.81653586104654E-17));
#2909=CARTESIAN_POINT('Origin',(0.,0.,0.));
#2910=CARTESIAN_POINT('Origin',(0.,-3.96,0.));
#2911=CARTESIAN_POINT('',(-0.32,-4.,-3.91886975727153E-17));
#2912=CARTESIAN_POINT('Origin',(0.,-4.,0.));
#2913=CARTESIAN_POINT('',(-0.36,-3.96,-4.40872847693047E-17));
#2914=CARTESIAN_POINT('Origin',(0.,-4.,0.));
#2915=CARTESIAN_POINT('Origin',(0.,0.462722715486149,0.));
#2916=CARTESIAN_POINT('',(-0.6175,0.53,-7.5621939847349E-17));
#2917=CARTESIAN_POINT('Origin',(0.,0.53,0.));
#2918=CARTESIAN_POINT('',(-0.750555349946514,0.453180457891261,-9.19165206894919E-17));
#2919=CARTESIAN_POINT('',(-0.734027674973257,0.462722715486149,-8.98924642641573E-17));
#2920=CARTESIAN_POINT('',(-0.375277674973257,0.453180457891261,0.65));
#2921=CARTESIAN_POINT('Ctrl Pts',(-0.375277674973257,0.45318045789126,0.65));
#2922=CARTESIAN_POINT('Ctrl Pts',(-0.562916512459968,0.561513791224244,
0.324999999999856));
#2923=CARTESIAN_POINT('Ctrl Pts',(-0.750555349946514,0.45318045789126,-9.19165206894919E-17));
#2924=CARTESIAN_POINT('',(0.375277674973257,0.453180457891261,0.65));
#2925=CARTESIAN_POINT('Ctrl Pts',(0.375277674973257,0.453180457891261,0.65));
#2926=CARTESIAN_POINT('Ctrl Pts',(-1.66922031752392E-13,0.561513791224244,
0.65));
#2927=CARTESIAN_POINT('Ctrl Pts',(-0.375277674973257,0.45318045789126,0.65));
#2928=CARTESIAN_POINT('',(0.750555349946514,0.453180457891261,0.));
#2929=CARTESIAN_POINT('Ctrl Pts',(0.750555349946514,0.453180457891261,0.));
#2930=CARTESIAN_POINT('Ctrl Pts',(0.562916512459802,0.561513791224244,0.325000000000144));
#2931=CARTESIAN_POINT('Ctrl Pts',(0.375277674973257,0.45318045789126,0.65));
#2932=CARTESIAN_POINT('',(0.375277674973257,0.453180457891261,-0.65));
#2933=CARTESIAN_POINT('Ctrl Pts',(0.375277674973257,0.45318045789126,-0.65));
#2934=CARTESIAN_POINT('Ctrl Pts',(0.562916512459968,0.561513791224244,-0.324999999999855));
#2935=CARTESIAN_POINT('Ctrl Pts',(0.750555349946514,0.453180457891261,0.));
#2936=CARTESIAN_POINT('',(-0.375277674973257,0.45318045789126,-0.65));
#2937=CARTESIAN_POINT('Ctrl Pts',(-0.375277674973257,0.453180457891261,
-0.65));
#2938=CARTESIAN_POINT('Ctrl Pts',(1.66866520601161E-13,0.561513791224244,
-0.65));
#2939=CARTESIAN_POINT('Ctrl Pts',(0.375277674973257,0.45318045789126,-0.65));
#2940=CARTESIAN_POINT('Ctrl Pts',(-0.750555349946514,0.453180457891261,
-9.19165206894919E-17));
#2941=CARTESIAN_POINT('Ctrl Pts',(-0.562916512459802,0.561513791224244,
-0.325000000000144));
#2942=CARTESIAN_POINT('Ctrl Pts',(-0.375277674973257,0.45318045789126,-0.65));
#2943=CARTESIAN_POINT('Origin',(0.375277674973257,0.,-0.65));
#2944=CARTESIAN_POINT('',(0.375277674973257,0.,-0.65));
#2945=CARTESIAN_POINT('',(0.375277674973257,0.,-0.65));
#2946=CARTESIAN_POINT('',(-0.375277674973257,0.,-0.65));
#2947=CARTESIAN_POINT('',(0.375277674973257,0.,-0.65));
#2948=CARTESIAN_POINT('',(-0.375277674973257,0.,-0.65));
#2949=CARTESIAN_POINT('Origin',(0.750555349946514,0.,0.));
#2950=CARTESIAN_POINT('',(0.750555349946514,0.,0.));
#2951=CARTESIAN_POINT('',(0.750555349946514,0.,0.));
#2952=CARTESIAN_POINT('',(0.750555349946514,0.,0.));
#2953=CARTESIAN_POINT('Origin',(0.375277674973257,0.,0.65));
#2954=CARTESIAN_POINT('',(0.375277674973257,0.,0.65));
#2955=CARTESIAN_POINT('',(0.375277674973257,0.,0.65));
#2956=CARTESIAN_POINT('',(0.375277674973257,0.,0.65));
#2957=CARTESIAN_POINT('Origin',(-0.375277674973257,0.,0.65));
#2958=CARTESIAN_POINT('',(-0.375277674973257,0.,0.65));
#2959=CARTESIAN_POINT('',(-0.375277674973257,0.,0.65));
#2960=CARTESIAN_POINT('',(-0.375277674973257,0.,0.65));
#2961=CARTESIAN_POINT('Origin',(-0.750555349946514,0.,-9.19165206894919E-17));
#2962=CARTESIAN_POINT('',(-0.750555349946514,0.,-9.19165206894919E-17));
#2963=CARTESIAN_POINT('',(-0.750555349946514,0.,-9.19165206894919E-17));
#2964=CARTESIAN_POINT('',(-0.750555349946514,0.,-9.19165206894919E-17));
#2965=CARTESIAN_POINT('Origin',(-0.375277674973257,0.,-0.65));
#2966=CARTESIAN_POINT('',(-0.375277674973257,0.,-0.65));
#2967=CARTESIAN_POINT('Origin',(0.,0.53,-1.11022302462516E-16));
#2968=CARTESIAN_POINT('Origin',(0.,0.,-1.11022302462516E-16));
#2969=CARTESIAN_POINT('',(0.,0.,0.));
#2970=CARTESIAN_POINT('',(0.,0.,0.));
#2971=CARTESIAN_POINT('',(0.,0.,0.));
#2972=CARTESIAN_POINT('',(0.5,-1.5,0.));
#2973=CARTESIAN_POINT('',(0.5,1.5,0.));
#2974=CARTESIAN_POINT('',(2.5,-1.5,0.));
#2975=CARTESIAN_POINT('',(2.5,1.5,0.));
#2976=CARTESIAN_POINT('',(1.5,0.,4.));
#2977=CARTESIAN_POINT('',(1.5,0.,4.16));
#2978=CARTESIAN_POINT('',(0.,0.,0.));
#2979=UNCERTAINTY_MEASURE_WITH_UNIT(LENGTH_MEASURE(0.001),#2997,
'DISTANCE_ACCURACY_VALUE',
'Maximum model space distance between geometric entities at asserted c
onnectivities');
#2980=UNCERTAINTY_MEASURE_WITH_UNIT(LENGTH_MEASURE(0.001),#2997,
'DISTANCE_ACCURACY_VALUE',
'Maximum model space distance between geometric entities at asserted c
onnectivities');
#2981=UNCERTAINTY_MEASURE_WITH_UNIT(LENGTH_MEASURE(0.001),#2997,
'DISTANCE_ACCURACY_VALUE',
'Maximum model space distance between geometric entities at asserted c
onnectivities');
#2982=UNCERTAINTY_MEASURE_WITH_UNIT(LENGTH_MEASURE(0.001),#2997,
'DISTANCE_ACCURACY_VALUE',
'Maximum model space distance between geometric entities at asserted c
onnectivities');
#2983=UNCERTAINTY_MEASURE_WITH_UNIT(LENGTH_MEASURE(0.001),#2997,
'DISTANCE_ACCURACY_VALUE',
'Maximum model space distance between geometric entities at asserted c
onnectivities');
#2984=UNCERTAINTY_MEASURE_WITH_UNIT(LENGTH_MEASURE(0.001),#2997,
'DISTANCE_ACCURACY_VALUE',
'Maximum model space distance between geometric entities at asserted c
onnectivities');
#2985=UNCERTAINTY_MEASURE_WITH_UNIT(LENGTH_MEASURE(0.001),#2997,
'DISTANCE_ACCURACY_VALUE',
'Maximum model space distance between geometric entities at asserted c
onnectivities');
#2986=UNCERTAINTY_MEASURE_WITH_UNIT(LENGTH_MEASURE(0.001),#2997,
'DISTANCE_ACCURACY_VALUE',
'Maximum model space distance between geometric entities at asserted c
onnectivities');
#2987=UNCERTAINTY_MEASURE_WITH_UNIT(LENGTH_MEASURE(0.001),#2997,
'DISTANCE_ACCURACY_VALUE',
'Maximum model space distance between geometric entities at asserted c
onnectivities');
#2988=(
GEOMETRIC_REPRESENTATION_CONTEXT(3)
GLOBAL_UNCERTAINTY_ASSIGNED_CONTEXT((#2979))
GLOBAL_UNIT_ASSIGNED_CONTEXT((#2997,#2999,#3000))
REPRESENTATION_CONTEXT('','3D')
);
#2989=(
GEOMETRIC_REPRESENTATION_CONTEXT(3)
GLOBAL_UNCERTAINTY_ASSIGNED_CONTEXT((#2980))
GLOBAL_UNIT_ASSIGNED_CONTEXT((#2997,#2999,#3000))
REPRESENTATION_CONTEXT('','3D')
);
#2990=(
GEOMETRIC_REPRESENTATION_CONTEXT(3)
GLOBAL_UNCERTAINTY_ASSIGNED_CONTEXT((#2981))
GLOBAL_UNIT_ASSIGNED_CONTEXT((#2997,#2999,#3000))
REPRESENTATION_CONTEXT('','3D')
);
#2991=(
GEOMETRIC_REPRESENTATION_CONTEXT(3)
GLOBAL_UNCERTAINTY_ASSIGNED_CONTEXT((#2982))
GLOBAL_UNIT_ASSIGNED_CONTEXT((#2997,#2999,#3000))
REPRESENTATION_CONTEXT('','3D')
);
#2992=(
GEOMETRIC_REPRESENTATION_CONTEXT(3)
GLOBAL_UNCERTAINTY_ASSIGNED_CONTEXT((#2983))
GLOBAL_UNIT_ASSIGNED_CONTEXT((#2997,#2999,#3000))
REPRESENTATION_CONTEXT('','3D')
);
#2993=(
GEOMETRIC_REPRESENTATION_CONTEXT(3)
GLOBAL_UNCERTAINTY_ASSIGNED_CONTEXT((#2984))
GLOBAL_UNIT_ASSIGNED_CONTEXT((#2997,#2999,#3000))
REPRESENTATION_CONTEXT('','3D')
);
#2994=(
GEOMETRIC_REPRESENTATION_CONTEXT(3)
GLOBAL_UNCERTAINTY_ASSIGNED_CONTEXT((#2985))
GLOBAL_UNIT_ASSIGNED_CONTEXT((#2997,#2999,#3000))
REPRESENTATION_CONTEXT('','3D')
);
#2995=(
GEOMETRIC_REPRESENTATION_CONTEXT(3)
GLOBAL_UNCERTAINTY_ASSIGNED_CONTEXT((#2986))
GLOBAL_UNIT_ASSIGNED_CONTEXT((#2997,#2999,#3000))
REPRESENTATION_CONTEXT('','3D')
);
#2996=(
GEOMETRIC_REPRESENTATION_CONTEXT(3)
GLOBAL_UNCERTAINTY_ASSIGNED_CONTEXT((#2987))
GLOBAL_UNIT_ASSIGNED_CONTEXT((#2997,#2999,#3000))
REPRESENTATION_CONTEXT('','3D')
);
#2997=(
LENGTH_UNIT()
NAMED_UNIT(*)
SI_UNIT(.CENTI.,.METRE.)
);
#2998=(
LENGTH_UNIT()
NAMED_UNIT(*)
SI_UNIT($,.METRE.)
);
#2999=(
NAMED_UNIT(*)
PLANE_ANGLE_UNIT()
SI_UNIT($,.RADIAN.)
);
#3000=(
NAMED_UNIT(*)
SI_UNIT($,.STERADIAN.)
SOLID_ANGLE_UNIT()
);
#3001=SHAPE_DEFINITION_REPRESENTATION(#3009,#3027);
#3002=SHAPE_DEFINITION_REPRESENTATION(#3010,#3028);
#3003=SHAPE_DEFINITION_REPRESENTATION(#3011,#3029);
#3004=SHAPE_DEFINITION_REPRESENTATION(#3012,#3030);
#3005=SHAPE_DEFINITION_REPRESENTATION(#3013,#3031);
#3006=SHAPE_DEFINITION_REPRESENTATION(#3014,#3032);
#3007=SHAPE_DEFINITION_REPRESENTATION(#3015,#3033);
#3008=SHAPE_DEFINITION_REPRESENTATION(#3016,#3034);
#3009=PRODUCT_DEFINITION_SHAPE('',$,#3036);
#3010=PRODUCT_DEFINITION_SHAPE('',$,#3037);
#3011=PRODUCT_DEFINITION_SHAPE('',$,#3038);
#3012=PRODUCT_DEFINITION_SHAPE('',$,#3039);
#3013=PRODUCT_DEFINITION_SHAPE('',$,#3040);
#3014=PRODUCT_DEFINITION_SHAPE('',$,#3041);
#3015=PRODUCT_DEFINITION_SHAPE('',$,#3042);
#3016=PRODUCT_DEFINITION_SHAPE('',$,#3043);
#3017=PRODUCT_DEFINITION_SHAPE($,$,#41);
#3018=PRODUCT_DEFINITION_SHAPE($,$,#42);
#3019=PRODUCT_DEFINITION_SHAPE($,$,#43);
#3020=PRODUCT_DEFINITION_SHAPE($,$,#44);
#3021=PRODUCT_DEFINITION_SHAPE($,$,#45);
#3022=PRODUCT_DEFINITION_SHAPE($,$,#46);
#3023=PRODUCT_DEFINITION_SHAPE($,$,#47);
#3024=PRODUCT_DEFINITION_SHAPE($,$,#48);
#3025=PRODUCT_DEFINITION_SHAPE($,$,#49);
#3026=PRODUCT_DEFINITION_SHAPE($,$,#50);
#3027=SHAPE_REPRESENTATION('',(#1782,#1981),#2988);
#3028=SHAPE_REPRESENTATION('',(#1783,#1972,#1973,#1974,#1975,#1976,#1977,
#1978,#1979,#1980),#2989);
#3029=SHAPE_REPRESENTATION('',(#1784),#2990);
#3030=SHAPE_REPRESENTATION('',(#1881),#2991);
#3031=SHAPE_REPRESENTATION('',(#1907),#2992);
#3032=SHAPE_REPRESENTATION('',(#1922),#2993);
#3033=SHAPE_REPRESENTATION('',(#1946),#2994);
#3034=SHAPE_REPRESENTATION('',(#1955),#2995);
#3035=PRODUCT_DEFINITION_CONTEXT('part definition',#3061,'design');
#3036=PRODUCT_DEFINITION('PAT-071',
'PAT-071',#3044,#3035);
#3037=PRODUCT_DEFINITION('Fixture grid and wedge clamp',
'Fixture grid and wedge clamp',#3045,#3035);
#3038=PRODUCT_DEFINITION('Fixture grid plate','Fixture grid plate',#3046,
#3035);
#3039=PRODUCT_DEFINITION('Inclined clamp support',
'Inclined clamp support',#3047,#3035);
#3040=PRODUCT_DEFINITION('Wedge clamping shoe','Wedge clamping shoe',#3048,
#3035);
#3041=PRODUCT_DEFINITION('M5x14 Cap Screw','M5x14 Cap Screw',#3049,#3035);
#3042=PRODUCT_DEFINITION('Flat Washer - M8','Flat Washer - M8',#3050,#3035);
#3043=PRODUCT_DEFINITION('Hex Bolt - M8x40','Hex Bolt - M8x40',#3051,#3035);
#3044=PRODUCT_DEFINITION_FORMATION('',$,#3063);
#3045=PRODUCT_DEFINITION_FORMATION('',$,#3064);
#3046=PRODUCT_DEFINITION_FORMATION('',$,#3065);
#3047=PRODUCT_DEFINITION_FORMATION('',$,#3066);
#3048=PRODUCT_DEFINITION_FORMATION('',$,#3067);
#3049=PRODUCT_DEFINITION_FORMATION('',$,#3068);
#3050=PRODUCT_DEFINITION_FORMATION('',$,#3069);
#3051=PRODUCT_DEFINITION_FORMATION('',$,#3070);
#3052=PRODUCT_RELATED_PRODUCT_CATEGORY(
'PAT-071','PAT-071',(#3063));
#3053=PRODUCT_RELATED_PRODUCT_CATEGORY('Fixture grid and wedge clamp',
'Fixture grid and wedge clamp',(#3064));
#3054=PRODUCT_RELATED_PRODUCT_CATEGORY('Fixture grid plate',
'Fixture grid plate',(#3065));
#3055=PRODUCT_RELATED_PRODUCT_CATEGORY('Inclined clamp support',
'Inclined clamp support',(#3066));
#3056=PRODUCT_RELATED_PRODUCT_CATEGORY('Wedge clamping shoe',
'Wedge clamping shoe',(#3067));
#3057=PRODUCT_RELATED_PRODUCT_CATEGORY('M5x14 Cap Screw',
'M5x14 Cap Screw',(#3068));
#3058=PRODUCT_RELATED_PRODUCT_CATEGORY('Flat Washer - M8',
'Flat Washer - M8',(#3069));
#3059=PRODUCT_RELATED_PRODUCT_CATEGORY('Hex Bolt - M8x40',
'Hex Bolt - M8x40',(#3070));
#3060=APPLICATION_PROTOCOL_DEFINITION('international standard',
'automotive_design',2009,#3061);
#3061=APPLICATION_CONTEXT(
'Core Data for Automotive Mechanical Design Process');
#3062=PRODUCT_CONTEXT('part definition',#3061,'mechanical');
#3063=PRODUCT('PAT-071',
'PAT-071','PAT-071',(#3062));
#3064=PRODUCT('Fixture grid and wedge clamp',
'Fixture grid and wedge clamp','Fixture grid and wedge clamp',(#3062));
#3065=PRODUCT('Fixture grid plate','Fixture grid plate',
'Fixture grid plate',(#3062));
#3066=PRODUCT('Inclined clamp support','Inclined clamp support',
'Inclined clamp support',(#3062));
#3067=PRODUCT('Wedge clamping shoe','Wedge clamping shoe',
'Wedge clamping shoe',(#3062));
#3068=PRODUCT('M5x14 Cap Screw','M5x14 Cap Screw','M5x14 Cap Screw',(#3062));
#3069=PRODUCT('Flat Washer - M8','Flat Washer - M8','Flat Washer - M8',
(#3062));
#3070=PRODUCT('Hex Bolt - M8x40','Hex Bolt - M8x40','Hex Bolt - M8x40',
(#3062));
#3071=PRESENTATION_STYLE_ASSIGNMENT((#3075));
#3072=PRESENTATION_STYLE_ASSIGNMENT((#3076));
#3073=PRESENTATION_STYLE_ASSIGNMENT((#3077));
#3074=PRESENTATION_STYLE_ASSIGNMENT((#3078));
#3075=SURFACE_STYLE_USAGE(.BOTH.,#3079);
#3076=SURFACE_STYLE_USAGE(.BOTH.,#3080);
#3077=SURFACE_STYLE_USAGE(.BOTH.,#3081);
#3078=SURFACE_STYLE_USAGE(.BOTH.,#3082);
#3079=SURFACE_SIDE_STYLE('',(#3083));
#3080=SURFACE_SIDE_STYLE('',(#3084));
#3081=SURFACE_SIDE_STYLE('',(#3085));
#3082=SURFACE_SIDE_STYLE('',(#3086));
#3083=SURFACE_STYLE_FILL_AREA(#3087);
#3084=SURFACE_STYLE_FILL_AREA(#3088);
#3085=SURFACE_STYLE_FILL_AREA(#3089);
#3086=SURFACE_STYLE_FILL_AREA(#3090);
#3087=FILL_AREA_STYLE('Steel - Satin',(#3091));
#3088=FILL_AREA_STYLE('CAD Library Painted - Engineering blue',(#3092));
#3089=FILL_AREA_STYLE('CAD Library Painted - Graphite',(#3093));
#3090=FILL_AREA_STYLE('CAD Library Painted - Steel gray',(#3094));
#3091=FILL_AREA_STYLE_COLOUR('Steel - Satin',#3095);
#3092=FILL_AREA_STYLE_COLOUR('CAD Library Painted - Engineering blue',#3096);
#3093=FILL_AREA_STYLE_COLOUR('CAD Library Painted - Graphite',#3097);
#3094=FILL_AREA_STYLE_COLOUR('CAD Library Painted - Steel gray',#3098);
#3095=COLOUR_RGB('Steel - Satin',0.627450980392157,0.627450980392157,0.627450980392157);
#3096=COLOUR_RGB('CAD Library Painted - Engineering blue',0.12156862745098,
0.356862745098039,0.6);
#3097=COLOUR_RGB('CAD Library Painted - Graphite',0.0980392156862745,0.109803921568627,
0.125490196078431);
#3098=COLOUR_RGB('CAD Library Painted - Steel gray',0.592156862745098,0.631372549019608,
0.67843137254902);
#3099=COLOUR_RGB('Dark Blue',0.08,0.2,0.34);
#3100=FILL_AREA_STYLE_COLOUR('',#3099);
#3101=FILL_AREA_STYLE('',(#3100));
#3102=SURFACE_STYLE_FILL_AREA(#3101);
#3103=SURFACE_SIDE_STYLE('',(#3102));
#3104=SURFACE_STYLE_USAGE(.BOTH.,#3103);
#3105=PRESENTATION_STYLE_ASSIGNMENT((#3104));
#3106=COLOUR_RGB('Light Blue',0.38,0.62,0.78);
#3107=FILL_AREA_STYLE_COLOUR('',#3106);
#3108=FILL_AREA_STYLE('',(#3107));
#3109=SURFACE_STYLE_FILL_AREA(#3108);
#3110=SURFACE_SIDE_STYLE('',(#3109));
#3111=SURFACE_STYLE_USAGE(.BOTH.,#3110);
#3112=PRESENTATION_STYLE_ASSIGNMENT((#3111));
#3113=COLOUR_RGB('Sky Blue',0.24,0.69,0.87);
#3114=FILL_AREA_STYLE_COLOUR('',#3113);
#3115=FILL_AREA_STYLE('',(#3114));
#3116=SURFACE_STYLE_FILL_AREA(#3115);
#3117=SURFACE_SIDE_STYLE('',(#3116));
#3118=SURFACE_STYLE_USAGE(.BOTH.,#3117);
#3119=PRESENTATION_STYLE_ASSIGNMENT((#3118));
#3120=COLOUR_RGB('Grey',0.48,0.52,0.57);
#3121=FILL_AREA_STYLE_COLOUR('',#3120);
#3122=FILL_AREA_STYLE('',(#3121));
#3123=SURFACE_STYLE_FILL_AREA(#3122);
#3124=SURFACE_SIDE_STYLE('',(#3123));
#3125=SURFACE_STYLE_USAGE(.BOTH.,#3124);
#3126=PRESENTATION_STYLE_ASSIGNMENT((#3125));
#3127=COLOUR_RGB('Black',0.12,0.14,0.17);
#3128=FILL_AREA_STYLE_COLOUR('',#3127);
#3129=FILL_AREA_STYLE('',(#3128));
#3130=SURFACE_STYLE_FILL_AREA(#3129);
#3131=SURFACE_SIDE_STYLE('',(#3130));
#3132=SURFACE_STYLE_USAGE(.BOTH.,#3131);
#3133=PRESENTATION_STYLE_ASSIGNMENT((#3132));
#3134=COLOUR_RGB('Off White',0.89,0.88,0.83);
#3135=FILL_AREA_STYLE_COLOUR('',#3134);
#3136=FILL_AREA_STYLE('',(#3135));
#3137=SURFACE_STYLE_FILL_AREA(#3136);
#3138=SURFACE_SIDE_STYLE('',(#3137));
#3139=SURFACE_STYLE_USAGE(.BOTH.,#3138);
#3140=PRESENTATION_STYLE_ASSIGNMENT((#3139));
ENDSEC;
END-ISO-10303-21;
